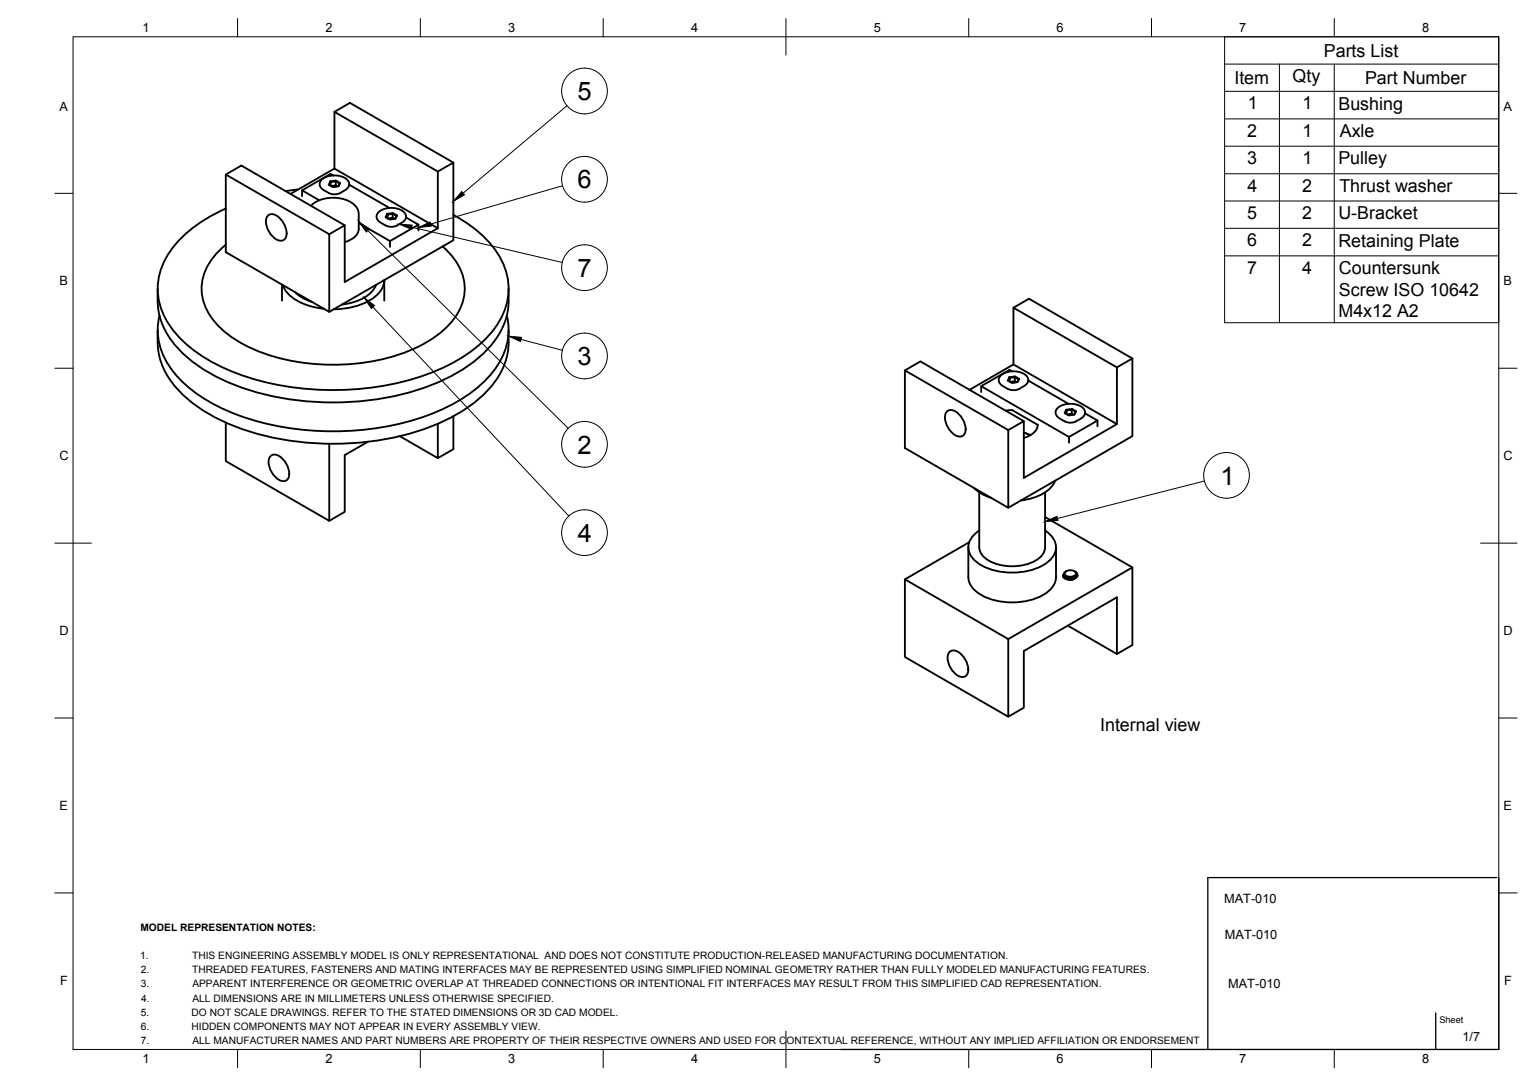
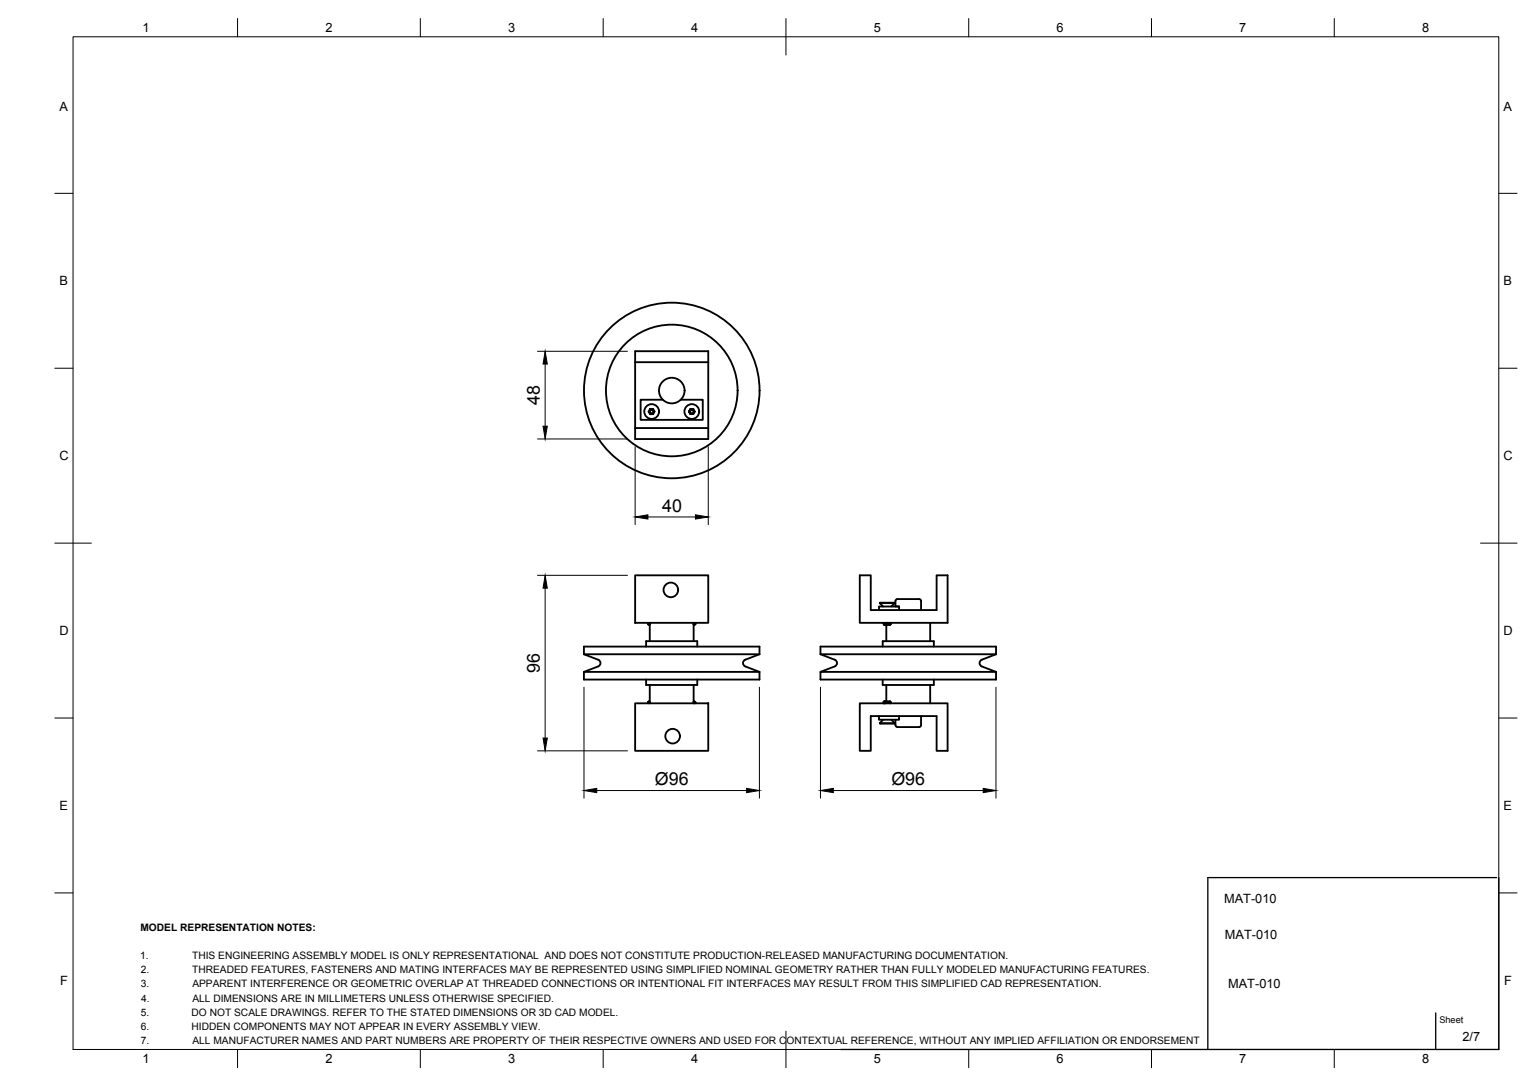
ISO-10303-21;
HEADER;
/* Generated by software containing ST-Developer
 * from STEP Tools, Inc. (www.steptools.com) 
 */

FILE_DESCRIPTION(
/* description */ ('STEP AP214'),
/* implementation_level */ '2;1');

FILE_NAME(
/* name */ 'MAT-010.step',
/* time_stamp */ '2026-11-14T05:50:49-08:00',
/* author */ (''),
/* organization */ (''),
/* preprocessor_version */ 'ST-DEVELOPER v20.2',
/* originating_system */ 'Autodesk Translation Framework v15.17.0.0',
/* authorisation */ '');

FILE_SCHEMA (('AUTOMOTIVE_DESIGN { 1 0 10303 214 3 1 1 }'));
ENDSEC;

DATA;
#10=MECHANICAL_DESIGN_GEOMETRIC_PRESENTATION_REPRESENTATION('',(#157,#158,
#159,#160,#161,#162,#163),#9903);
#11=ITEM_DEFINED_TRANSFORMATION($,$,#2108,#2305);
#12=ITEM_DEFINED_TRANSFORMATION($,$,#2117,#2306);
#13=ITEM_DEFINED_TRANSFORMATION($,$,#2141,#2307);
#14=ITEM_DEFINED_TRANSFORMATION($,$,#2189,#2308);
#15=ITEM_DEFINED_TRANSFORMATION($,$,#2198,#2309);
#16=ITEM_DEFINED_TRANSFORMATION($,$,#2221,#2310);
#17=ITEM_DEFINED_TRANSFORMATION($,$,#2234,#2311);
#18=ITEM_DEFINED_TRANSFORMATION($,$,#2189,#2312);
#19=ITEM_DEFINED_TRANSFORMATION($,$,#2198,#2313);
#20=ITEM_DEFINED_TRANSFORMATION($,$,#2221,#2314);
#21=ITEM_DEFINED_TRANSFORMATION($,$,#2234,#2315);
#22=ITEM_DEFINED_TRANSFORMATION($,$,#2234,#2316);
#23=ITEM_DEFINED_TRANSFORMATION($,$,#2234,#2317);
#24=(
REPRESENTATION_RELATIONSHIP($,$,#9938,#9937)
REPRESENTATION_RELATIONSHIP_WITH_TRANSFORMATION(#11)
SHAPE_REPRESENTATION_RELATIONSHIP()
);
#25=(
REPRESENTATION_RELATIONSHIP($,$,#9939,#9937)
REPRESENTATION_RELATIONSHIP_WITH_TRANSFORMATION(#12)
SHAPE_REPRESENTATION_RELATIONSHIP()
);
#26=(
REPRESENTATION_RELATIONSHIP($,$,#9940,#9937)
REPRESENTATION_RELATIONSHIP_WITH_TRANSFORMATION(#13)
SHAPE_REPRESENTATION_RELATIONSHIP()
);
#27=(
REPRESENTATION_RELATIONSHIP($,$,#9941,#9937)
REPRESENTATION_RELATIONSHIP_WITH_TRANSFORMATION(#14)
SHAPE_REPRESENTATION_RELATIONSHIP()
);
#28=(
REPRESENTATION_RELATIONSHIP($,$,#9942,#9937)
REPRESENTATION_RELATIONSHIP_WITH_TRANSFORMATION(#15)
SHAPE_REPRESENTATION_RELATIONSHIP()
);
#29=(
REPRESENTATION_RELATIONSHIP($,$,#9943,#9937)
REPRESENTATION_RELATIONSHIP_WITH_TRANSFORMATION(#16)
SHAPE_REPRESENTATION_RELATIONSHIP()
);
#30=(
REPRESENTATION_RELATIONSHIP($,$,#9944,#9937)
REPRESENTATION_RELATIONSHIP_WITH_TRANSFORMATION(#17)
SHAPE_REPRESENTATION_RELATIONSHIP()
);
#31=(
REPRESENTATION_RELATIONSHIP($,$,#9941,#9937)
REPRESENTATION_RELATIONSHIP_WITH_TRANSFORMATION(#18)
SHAPE_REPRESENTATION_RELATIONSHIP()
);
#32=(
REPRESENTATION_RELATIONSHIP($,$,#9942,#9937)
REPRESENTATION_RELATIONSHIP_WITH_TRANSFORMATION(#19)
SHAPE_REPRESENTATION_RELATIONSHIP()
);
#33=(
REPRESENTATION_RELATIONSHIP($,$,#9943,#9937)
REPRESENTATION_RELATIONSHIP_WITH_TRANSFORMATION(#20)
SHAPE_REPRESENTATION_RELATIONSHIP()
);
#34=(
REPRESENTATION_RELATIONSHIP($,$,#9944,#9937)
REPRESENTATION_RELATIONSHIP_WITH_TRANSFORMATION(#21)
SHAPE_REPRESENTATION_RELATIONSHIP()
);
#35=(
REPRESENTATION_RELATIONSHIP($,$,#9944,#9937)
REPRESENTATION_RELATIONSHIP_WITH_TRANSFORMATION(#22)
SHAPE_REPRESENTATION_RELATIONSHIP()
);
#36=(
REPRESENTATION_RELATIONSHIP($,$,#9944,#9937)
REPRESENTATION_RELATIONSHIP_WITH_TRANSFORMATION(#23)
SHAPE_REPRESENTATION_RELATIONSHIP()
);
#37=CONTEXT_DEPENDENT_SHAPE_REPRESENTATION(#24,#9924);
#38=CONTEXT_DEPENDENT_SHAPE_REPRESENTATION(#25,#9925);
#39=CONTEXT_DEPENDENT_SHAPE_REPRESENTATION(#26,#9926);
#40=CONTEXT_DEPENDENT_SHAPE_REPRESENTATION(#27,#9927);
#41=CONTEXT_DEPENDENT_SHAPE_REPRESENTATION(#28,#9928);
#42=CONTEXT_DEPENDENT_SHAPE_REPRESENTATION(#29,#9929);
#43=CONTEXT_DEPENDENT_SHAPE_REPRESENTATION(#30,#9930);
#44=CONTEXT_DEPENDENT_SHAPE_REPRESENTATION(#31,#9931);
#45=CONTEXT_DEPENDENT_SHAPE_REPRESENTATION(#32,#9932);
#46=CONTEXT_DEPENDENT_SHAPE_REPRESENTATION(#33,#9933);
#47=CONTEXT_DEPENDENT_SHAPE_REPRESENTATION(#34,#9934);
#48=CONTEXT_DEPENDENT_SHAPE_REPRESENTATION(#35,#9935);
#49=CONTEXT_DEPENDENT_SHAPE_REPRESENTATION(#36,#9936);
#50=NEXT_ASSEMBLY_USAGE_OCCURRENCE('Bushing:1','Bushing:1','Bushing:1',
#9946,#9947,'Bushing:1');
#51=NEXT_ASSEMBLY_USAGE_OCCURRENCE('Axle:1','Axle:1','Axle:1',#9946,#9948,
'Axle:1');
#52=NEXT_ASSEMBLY_USAGE_OCCURRENCE('Pulley:1','Pulley:1','Pulley:1',#9946,
#9949,'Pulley:1');
#53=NEXT_ASSEMBLY_USAGE_OCCURRENCE('Thrust Washer:1','Thrust Washer:1',
'Thrust Washer:1',#9946,#9950,'Thrust Washer:1');
#54=NEXT_ASSEMBLY_USAGE_OCCURRENCE('U-Bracket:1','U-Bracket:1',
'U-Bracket:1',#9946,#9951,'U-Bracket:1');
#55=NEXT_ASSEMBLY_USAGE_OCCURRENCE('Retaining Plate:1',
'Retaining Plate:1','Retaining Plate:1',#9946,#9952,'Retaining Plate:1');
#56=NEXT_ASSEMBLY_USAGE_OCCURRENCE(
'Countersunk Screw ISO 10642 M4x12 A2:1',
'Countersunk Screw ISO 10642 M4x12 A2:1',
'Countersunk Screw ISO 10642 M4x12 A2:1',#9946,#9953,
'Countersunk Screw ISO 10642 M4x12 A2:1');
#57=NEXT_ASSEMBLY_USAGE_OCCURRENCE('Thrust Washer:2','Thrust Washer:2',
'Thrust Washer:2',#9946,#9950,'Thrust Washer:2');
#58=NEXT_ASSEMBLY_USAGE_OCCURRENCE('U-Bracket:2','U-Bracket:2',
'U-Bracket:2',#9946,#9951,'U-Bracket:2');
#59=NEXT_ASSEMBLY_USAGE_OCCURRENCE('Retaining Plate:2',
'Retaining Plate:2','Retaining Plate:2',#9946,#9952,'Retaining Plate:2');
#60=NEXT_ASSEMBLY_USAGE_OCCURRENCE(
'Countersunk Screw ISO 10642 M4x12 A2:2',
'Countersunk Screw ISO 10642 M4x12 A2:2',
'Countersunk Screw ISO 10642 M4x12 A2:2',#9946,#9953,
'Countersunk Screw ISO 10642 M4x12 A2:2');
#61=NEXT_ASSEMBLY_USAGE_OCCURRENCE(
'Countersunk Screw ISO 10642 M4x12 A2:3',
'Countersunk Screw ISO 10642 M4x12 A2:3',
'Countersunk Screw ISO 10642 M4x12 A2:3',#9946,#9953,
'Countersunk Screw ISO 10642 M4x12 A2:3');
#62=NEXT_ASSEMBLY_USAGE_OCCURRENCE(
'Countersunk Screw ISO 10642 M4x12 A2:4',
'Countersunk Screw ISO 10642 M4x12 A2:4',
'Countersunk Screw ISO 10642 M4x12 A2:4',#9946,#9953,
'Countersunk Screw ISO 10642 M4x12 A2:4');
#63=(
BOUNDED_SURFACE()
B_SPLINE_SURFACE(1,2,((#4642,#4643,#4644,#4645,#4646,#4647,#4648,#4649,
#4650,#4651,#4652,#4653,#4654,#4655,#4656,#4657,#4658,#4659,#4660,#4661,
#4662,#4663,#4664,#4665,#4666,#4667,#4668,#4669,#4670,#4671,#4672,#4673,
#4674,#4675,#4676,#4677,#4678,#4679,#4680,#4681,#4682,#4683,#4684,#4685,
#4686,#4687,#4688,#4689,#4690,#4691,#4692,#4693,#4694,#4695,#4696,#4697,
#4698,#4699,#4700,#4701,#4702,#4703,#4704,#4705,#4706,#4707,#4708,#4709,
#4710,#4711,#4712,#4713,#4714,#4715,#4716,#4717,#4718,#4719,#4720,#4721,
#4722,#4723,#4724,#4725,#4726,#4727,#4728,#4729,#4730,#4731,#4732,#4733,
#4734,#4735,#4736,#4737,#4738,#4739,#4740,#4741,#4742,#4743,#4744,#4745,
#4746,#4747,#4748,#4749,#4750,#4751,#4752,#4753,#4754,#4755,#4756,#4757,
#4758,#4759,#4760,#4761,#4762,#4763,#4764,#4765,#4766,#4767,#4768,#4769,
#4770,#4771,#4772,#4773,#4774,#4775,#4776,#4777,#4778,#4779,#4780,#4781,
#4782,#4783,#4784,#4785,#4786,#4787,#4788,#4789,#4790,#4791,#4792,#4793,
#4794,#4795,#4796,#4797,#4798,#4799,#4800,#4801,#4802,#4803,#4804,#4805,
#4806,#4807,#4808,#4809,#4810,#4811,#4812,#4813,#4814,#4815,#4816,#4817,
#4818,#4819,#4820,#4821,#4822,#4823,#4824,#4825,#4826,#4827,#4828,#4829,
#4830,#4831,#4832,#4833,#4834,#4835,#4836,#4837,#4838,#4839,#4840,#4841,
#4842,#4843,#4844,#4845,#4846,#4847,#4848,#4849,#4850,#4851,#4852,#4853,
#4854,#4855,#4856,#4857,#4858,#4859,#4860,#4861,#4862,#4863,#4864,#4865,
#4866,#4867,#4868,#4869,#4870,#4871,#4872,#4873,#4874,#4875,#4876,#4877,
#4878,#4879,#4880,#4881,#4882,#4883,#4884,#4885,#4886,#4887,#4888,#4889,
#4890,#4891,#4892,#4893,#4894,#4895,#4896,#4897,#4898,#4899,#4900,#4901,
#4902,#4903,#4904,#4905,#4906,#4907,#4908,#4909,#4910,#4911,#4912,#4913,
#4914,#4915,#4916,#4917,#4918,#4919,#4920,#4921,#4922,#4923,#4924,#4925,
#4926,#4927,#4928,#4929,#4930,#4931,#4932,#4933,#4934,#4935,#4936,#4937,
#4938,#4939,#4940,#4941,#4942,#4943,#4944,#4945,#4946,#4947,#4948,#4949,
#4950,#4951,#4952,#4953,#4954,#4955,#4956,#4957,#4958,#4959,#4960,#4961,
#4962,#4963,#4964,#4965,#4966,#4967,#4968,#4969,#4970,#4971,#4972,#4973,
#4974,#4975,#4976,#4977,#4978,#4979,#4980,#4981,#4982,#4983,#4984,#4985,
#4986,#4987,#4988,#4989,#4990,#4991,#4992,#4993,#4994,#4995,#4996,#4997,
#4998,#4999,#5000,#5001,#5002,#5003,#5004,#5005,#5006,#5007,#5008,#5009,
#5010,#5011,#5012,#5013,#5014,#5015,#5016,#5017,#5018,#5019,#5020,#5021,
#5022,#5023,#5024,#5025,#5026,#5027,#5028,#5029,#5030,#5031,#5032,#5033,
#5034,#5035,#5036,#5037,#5038,#5039,#5040,#5041,#5042,#5043,#5044,#5045,
#5046,#5047,#5048,#5049,#5050,#5051,#5052,#5053,#5054,#5055,#5056,#5057,
#5058,#5059,#5060,#5061,#5062,#5063,#5064,#5065,#5066,#5067,#5068,#5069,
#5070,#5071,#5072,#5073,#5074,#5075,#5076,#5077,#5078,#5079,#5080,#5081,
#5082,#5083,#5084,#5085,#5086,#5087,#5088,#5089,#5090,#5091,#5092,#5093,
#5094,#5095,#5096,#5097,#5098,#5099,#5100,#5101,#5102,#5103,#5104,#5105,
#5106,#5107,#5108,#5109,#5110,#5111,#5112,#5113,#5114,#5115,#5116,#5117,
#5118,#5119,#5120,#5121,#5122,#5123,#5124,#5125,#5126,#5127,#5128,#5129,
#5130,#5131,#5132,#5133,#5134,#5135,#5136,#5137,#5138,#5139,#5140,#5141,
#5142,#5143,#5144,#5145,#5146,#5147,#5148,#5149,#5150,#5151,#5152,#5153,
#5154,#5155,#5156,#5157,#5158,#5159,#5160,#5161,#5162,#5163,#5164,#5165,
#5166,#5167,#5168,#5169,#5170,#5171,#5172,#5173,#5174,#5175,#5176,#5177,
#5178,#5179,#5180,#5181,#5182,#5183,#5184,#5185,#5186,#5187,#5188,#5189,
#5190,#5191,#5192,#5193,#5194,#5195,#5196,#5197,#5198,#5199,#5200,#5201,
#5202,#5203,#5204,#5205,#5206,#5207,#5208,#5209,#5210,#5211,#5212,#5213,
#5214,#5215,#5216,#5217,#5218,#5219,#5220,#5221,#5222,#5223,#5224,#5225,
#5226,#5227,#5228,#5229,#5230,#5231,#5232,#5233,#5234,#5235,#5236,#5237,
#5238,#5239,#5240,#5241,#5242,#5243,#5244,#5245,#5246,#5247,#5248,#5249,
#5250,#5251,#5252,#5253,#5254,#5255,#5256,#5257,#5258,#5259,#5260,#5261,
#5262,#5263,#5264,#5265,#5266,#5267,#5268,#5269,#5270,#5271,#5272,#5273,
#5274,#5275,#5276,#5277,#5278,#5279,#5280,#5281,#5282,#5283,#5284,#5285,
#5286,#5287,#5288,#5289,#5290,#5291,#5292,#5293,#5294,#5295,#5296,#5297,
#5298,#5299,#5300,#5301,#5302,#5303,#5304,#5305,#5306,#5307,#5308,#5309,
#5310,#5311,#5312,#5313,#5314,#5315,#5316,#5317,#5318,#5319,#5320,#5321,
#5322,#5323,#5324,#5325,#5326,#5327,#5328,#5329,#5330,#5331,#5332,#5333,
#5334,#5335,#5336,#5337,#5338,#5339,#5340,#5341,#5342,#5343,#5344,#5345,
#5346,#5347,#5348,#5349,#5350,#5351,#5352,#5353,#5354,#5355,#5356,#5357,
#5358,#5359,#5360,#5361,#5362,#5363,#5364,#5365,#5366,#5367,#5368,#5369,
#5370,#5371,#5372,#5373,#5374,#5375,#5376,#5377,#5378,#5379,#5380,#5381,
#5382,#5383,#5384,#5385,#5386,#5387,#5388,#5389,#5390,#5391,#5392,#5393,
#5394,#5395,#5396,#5397,#5398,#5399,#5400,#5401,#5402,#5403,#5404,#5405,
#5406,#5407,#5408,#5409,#5410,#5411,#5412,#5413,#5414,#5415,#5416,#5417,
#5418,#5419,#5420,#5421,#5422,#5423,#5424,#5425,#5426,#5427,#5428,#5429,
#5430,#5431,#5432,#5433,#5434,#5435,#5436,#5437,#5438,#5439,#5440,#5441,
#5442,#5443,#5444,#5445,#5446,#5447,#5448,#5449,#5450,#5451,#5452,#5453,
#5454,#5455,#5456,#5457,#5458,#5459,#5460,#5461,#5462,#5463,#5464,#5465,
#5466,#5467,#5468,#5469,#5470,#5471,#5472,#5473,#5474,#5475,#5476,#5477,
#5478,#5479,#5480,#5481,#5482,#5483,#5484,#5485,#5486,#5487,#5488,#5489,
#5490,#5491,#5492,#5493,#5494,#5495,#5496,#5497,#5498,#5499,#5500,#5501,
#5502,#5503,#5504,#5505,#5506,#5507,#5508,#5509,#5510,#5511,#5512,#5513,
#5514,#5515,#5516,#5517,#5518,#5519,#5520,#5521,#5522,#5523,#5524,#5525,
#5526,#5527,#5528,#5529,#5530,#5531,#5532,#5533,#5534,#5535,#5536,#5537,
#5538,#5539,#5540,#5541,#5542,#5543,#5544,#5545,#5546,#5547,#5548,#5549,
#5550,#5551,#5552,#5553,#5554,#5555,#5556,#5557,#5558,#5559,#5560,#5561,
#5562,#5563,#5564,#5565,#5566,#5567,#5568,#5569,#5570,#5571,#5572,#5573,
#5574,#5575,#5576,#5577,#5578,#5579,#5580,#5581,#5582,#5583,#5584,#5585,
#5586,#5587,#5588,#5589,#5590,#5591,#5592,#5593,#5594,#5595,#5596,#5597,
#5598,#5599,#5600,#5601,#5602,#5603,#5604,#5605,#5606,#5607,#5608,#5609,
#5610,#5611,#5612,#5613,#5614,#5615,#5616,#5617,#5618,#5619,#5620,#5621,
#5622,#5623,#5624,#5625,#5626,#5627,#5628,#5629,#5630,#5631,#5632,#5633,
#5634,#5635,#5636,#5637,#5638,#5639,#5640,#5641,#5642,#5643,#5644,#5645,
#5646,#5647,#5648,#5649,#5650,#5651,#5652,#5653,#5654,#5655,#5656,#5657,
#5658,#5659,#5660,#5661,#5662,#5663,#5664,#5665,#5666,#5667,#5668,#5669,
#5670,#5671,#5672,#5673,#5674,#5675,#5676,#5677,#5678,#5679,#5680,#5681,
#5682,#5683,#5684,#5685,#5686,#5687,#5688,#5689,#5690,#5691,#5692,#5693,
#5694,#5695,#5696,#5697,#5698,#5699,#5700,#5701,#5702,#5703,#5704,#5705,
#5706,#5707,#5708,#5709,#5710,#5711,#5712,#5713,#5714,#5715,#5716,#5717,
#5718,#5719,#5720,#5721,#5722,#5723,#5724,#5725,#5726,#5727,#5728,#5729,
#5730,#5731,#5732,#5733,#5734,#5735,#5736,#5737,#5738,#5739,#5740,#5741,
#5742,#5743,#5744,#5745,#5746,#5747,#5748,#5749,#5750,#5751,#5752,#5753,
#5754,#5755,#5756,#5757,#5758,#5759,#5760,#5761,#5762,#5763,#5764,#5765,
#5766,#5767,#5768,#5769,#5770,#5771,#5772,#5773,#5774,#5775,#5776,#5777,
#5778,#5779,#5780,#5781,#5782,#5783,#5784,#5785,#5786,#5787,#5788,#5789,
#5790,#5791,#5792,#5793,#5794,#5795,#5796,#5797,#5798,#5799,#5800,#5801,
#5802,#5803,#5804,#5805,#5806,#5807,#5808,#5809,#5810,#5811,#5812,#5813,
#5814,#5815,#5816,#5817,#5818,#5819,#5820,#5821,#5822,#5823,#5824,#5825,
#5826,#5827,#5828,#5829,#5830,#5831,#5832,#5833,#5834,#5835,#5836,#5837,
#5838,#5839,#5840,#5841,#5842,#5843,#5844,#5845,#5846,#5847,#5848,#5849,
#5850,#5851,#5852,#5853,#5854,#5855,#5856,#5857,#5858,#5859,#5860,#5861,
#5862,#5863,#5864,#5865,#5866,#5867,#5868,#5869,#5870,#5871,#5872,#5873,
#5874,#5875,#5876,#5877,#5878,#5879,#5880,#5881,#5882,#5883,#5884,#5885,
#5886,#5887,#5888,#5889,#5890,#5891,#5892,#5893,#5894,#5895,#5896,#5897,
#5898,#5899,#5900,#5901,#5902,#5903,#5904,#5905,#5906,#5907,#5908,#5909,
#5910,#5911,#5912),(#5913,#5914,#5915,#5916,#5917,#5918,#5919,#5920,#5921,
#5922,#5923,#5924,#5925,#5926,#5927,#5928,#5929,#5930,#5931,#5932,#5933,
#5934,#5935,#5936,#5937,#5938,#5939,#5940,#5941,#5942,#5943,#5944,#5945,
#5946,#5947,#5948,#5949,#5950,#5951,#5952,#5953,#5954,#5955,#5956,#5957,
#5958,#5959,#5960,#5961,#5962,#5963,#5964,#5965,#5966,#5967,#5968,#5969,
#5970,#5971,#5972,#5973,#5974,#5975,#5976,#5977,#5978,#5979,#5980,#5981,
#5982,#5983,#5984,#5985,#5986,#5987,#5988,#5989,#5990,#5991,#5992,#5993,
#5994,#5995,#5996,#5997,#5998,#5999,#6000,#6001,#6002,#6003,#6004,#6005,
#6006,#6007,#6008,#6009,#6010,#6011,#6012,#6013,#6014,#6015,#6016,#6017,
#6018,#6019,#6020,#6021,#6022,#6023,#6024,#6025,#6026,#6027,#6028,#6029,
#6030,#6031,#6032,#6033,#6034,#6035,#6036,#6037,#6038,#6039,#6040,#6041,
#6042,#6043,#6044,#6045,#6046,#6047,#6048,#6049,#6050,#6051,#6052,#6053,
#6054,#6055,#6056,#6057,#6058,#6059,#6060,#6061,#6062,#6063,#6064,#6065,
#6066,#6067,#6068,#6069,#6070,#6071,#6072,#6073,#6074,#6075,#6076,#6077,
#6078,#6079,#6080,#6081,#6082,#6083,#6084,#6085,#6086,#6087,#6088,#6089,
#6090,#6091,#6092,#6093,#6094,#6095,#6096,#6097,#6098,#6099,#6100,#6101,
#6102,#6103,#6104,#6105,#6106,#6107,#6108,#6109,#6110,#6111,#6112,#6113,
#6114,#6115,#6116,#6117,#6118,#6119,#6120,#6121,#6122,#6123,#6124,#6125,
#6126,#6127,#6128,#6129,#6130,#6131,#6132,#6133,#6134,#6135,#6136,#6137,
#6138,#6139,#6140,#6141,#6142,#6143,#6144,#6145,#6146,#6147,#6148,#6149,
#6150,#6151,#6152,#6153,#6154,#6155,#6156,#6157,#6158,#6159,#6160,#6161,
#6162,#6163,#6164,#6165,#6166,#6167,#6168,#6169,#6170,#6171,#6172,#6173,
#6174,#6175,#6176,#6177,#6178,#6179,#6180,#6181,#6182,#6183,#6184,#6185,
#6186,#6187,#6188,#6189,#6190,#6191,#6192,#6193,#6194,#6195,#6196,#6197,
#6198,#6199,#6200,#6201,#6202,#6203,#6204,#6205,#6206,#6207,#6208,#6209,
#6210,#6211,#6212,#6213,#6214,#6215,#6216,#6217,#6218,#6219,#6220,#6221,
#6222,#6223,#6224,#6225,#6226,#6227,#6228,#6229,#6230,#6231,#6232,#6233,
#6234,#6235,#6236,#6237,#6238,#6239,#6240,#6241,#6242,#6243,#6244,#6245,
#6246,#6247,#6248,#6249,#6250,#6251,#6252,#6253,#6254,#6255,#6256,#6257,
#6258,#6259,#6260,#6261,#6262,#6263,#6264,#6265,#6266,#6267,#6268,#6269,
#6270,#6271,#6272,#6273,#6274,#6275,#6276,#6277,#6278,#6279,#6280,#6281,
#6282,#6283,#6284,#6285,#6286,#6287,#6288,#6289,#6290,#6291,#6292,#6293,
#6294,#6295,#6296,#6297,#6298,#6299,#6300,#6301,#6302,#6303,#6304,#6305,
#6306,#6307,#6308,#6309,#6310,#6311,#6312,#6313,#6314,#6315,#6316,#6317,
#6318,#6319,#6320,#6321,#6322,#6323,#6324,#6325,#6326,#6327,#6328,#6329,
#6330,#6331,#6332,#6333,#6334,#6335,#6336,#6337,#6338,#6339,#6340,#6341,
#6342,#6343,#6344,#6345,#6346,#6347,#6348,#6349,#6350,#6351,#6352,#6353,
#6354,#6355,#6356,#6357,#6358,#6359,#6360,#6361,#6362,#6363,#6364,#6365,
#6366,#6367,#6368,#6369,#6370,#6371,#6372,#6373,#6374,#6375,#6376,#6377,
#6378,#6379,#6380,#6381,#6382,#6383,#6384,#6385,#6386,#6387,#6388,#6389,
#6390,#6391,#6392,#6393,#6394,#6395,#6396,#6397,#6398,#6399,#6400,#6401,
#6402,#6403,#6404,#6405,#6406,#6407,#6408,#6409,#6410,#6411,#6412,#6413,
#6414,#6415,#6416,#6417,#6418,#6419,#6420,#6421,#6422,#6423,#6424,#6425,
#6426,#6427,#6428,#6429,#6430,#6431,#6432,#6433,#6434,#6435,#6436,#6437,
#6438,#6439,#6440,#6441,#6442,#6443,#6444,#6445,#6446,#6447,#6448,#6449,
#6450,#6451,#6452,#6453,#6454,#6455,#6456,#6457,#6458,#6459,#6460,#6461,
#6462,#6463,#6464,#6465,#6466,#6467,#6468,#6469,#6470,#6471,#6472,#6473,
#6474,#6475,#6476,#6477,#6478,#6479,#6480,#6481,#6482,#6483,#6484,#6485,
#6486,#6487,#6488,#6489,#6490,#6491,#6492,#6493,#6494,#6495,#6496,#6497,
#6498,#6499,#6500,#6501,#6502,#6503,#6504,#6505,#6506,#6507,#6508,#6509,
#6510,#6511,#6512,#6513,#6514,#6515,#6516,#6517,#6518,#6519,#6520,#6521,
#6522,#6523,#6524,#6525,#6526,#6527,#6528,#6529,#6530,#6531,#6532,#6533,
#6534,#6535,#6536,#6537,#6538,#6539,#6540,#6541,#6542,#6543,#6544,#6545,
#6546,#6547,#6548,#6549,#6550,#6551,#6552,#6553,#6554,#6555,#6556,#6557,
#6558,#6559,#6560,#6561,#6562,#6563,#6564,#6565,#6566,#6567,#6568,#6569,
#6570,#6571,#6572,#6573,#6574,#6575,#6576,#6577,#6578,#6579,#6580,#6581,
#6582,#6583,#6584,#6585,#6586,#6587,#6588,#6589,#6590,#6591,#6592,#6593,
#6594,#6595,#6596,#6597,#6598,#6599,#6600,#6601,#6602,#6603,#6604,#6605,
#6606,#6607,#6608,#6609,#6610,#6611,#6612,#6613,#6614,#6615,#6616,#6617,
#6618,#6619,#6620,#6621,#6622,#6623,#6624,#6625,#6626,#6627,#6628,#6629,
#6630,#6631,#6632,#6633,#6634,#6635,#6636,#6637,#6638,#6639,#6640,#6641,
#6642,#6643,#6644,#6645,#6646,#6647,#6648,#6649,#6650,#6651,#6652,#6653,
#6654,#6655,#6656,#6657,#6658,#6659,#6660,#6661,#6662,#6663,#6664,#6665,
#6666,#6667,#6668,#6669,#6670,#6671,#6672,#6673,#6674,#6675,#6676,#6677,
#6678,#6679,#6680,#6681,#6682,#6683,#6684,#6685,#6686,#6687,#6688,#6689,
#6690,#6691,#6692,#6693,#6694,#6695,#6696,#6697,#6698,#6699,#6700,#6701,
#6702,#6703,#6704,#6705,#6706,#6707,#6708,#6709,#6710,#6711,#6712,#6713,
#6714,#6715,#6716,#6717,#6718,#6719,#6720,#6721,#6722,#6723,#6724,#6725,
#6726,#6727,#6728,#6729,#6730,#6731,#6732,#6733,#6734,#6735,#6736,#6737,
#6738,#6739,#6740,#6741,#6742,#6743,#6744,#6745,#6746,#6747,#6748,#6749,
#6750,#6751,#6752,#6753,#6754,#6755,#6756,#6757,#6758,#6759,#6760,#6761,
#6762,#6763,#6764,#6765,#6766,#6767,#6768,#6769,#6770,#6771,#6772,#6773,
#6774,#6775,#6776,#6777,#6778,#6779,#6780,#6781,#6782,#6783,#6784,#6785,
#6786,#6787,#6788,#6789,#6790,#6791,#6792,#6793,#6794,#6795,#6796,#6797,
#6798,#6799,#6800,#6801,#6802,#6803,#6804,#6805,#6806,#6807,#6808,#6809,
#6810,#6811,#6812,#6813,#6814,#6815,#6816,#6817,#6818,#6819,#6820,#6821,
#6822,#6823,#6824,#6825,#6826,#6827,#6828,#6829,#6830,#6831,#6832,#6833,
#6834,#6835,#6836,#6837,#6838,#6839,#6840,#6841,#6842,#6843,#6844,#6845,
#6846,#6847,#6848,#6849,#6850,#6851,#6852,#6853,#6854,#6855,#6856,#6857,
#6858,#6859,#6860,#6861,#6862,#6863,#6864,#6865,#6866,#6867,#6868,#6869,
#6870,#6871,#6872,#6873,#6874,#6875,#6876,#6877,#6878,#6879,#6880,#6881,
#6882,#6883,#6884,#6885,#6886,#6887,#6888,#6889,#6890,#6891,#6892,#6893,
#6894,#6895,#6896,#6897,#6898,#6899,#6900,#6901,#6902,#6903,#6904,#6905,
#6906,#6907,#6908,#6909,#6910,#6911,#6912,#6913,#6914,#6915,#6916,#6917,
#6918,#6919,#6920,#6921,#6922,#6923,#6924,#6925,#6926,#6927,#6928,#6929,
#6930,#6931,#6932,#6933,#6934,#6935,#6936,#6937,#6938,#6939,#6940,#6941,
#6942,#6943,#6944,#6945,#6946,#6947,#6948,#6949,#6950,#6951,#6952,#6953,
#6954,#6955,#6956,#6957,#6958,#6959,#6960,#6961,#6962,#6963,#6964,#6965,
#6966,#6967,#6968,#6969,#6970,#6971,#6972,#6973,#6974,#6975,#6976,#6977,
#6978,#6979,#6980,#6981,#6982,#6983,#6984,#6985,#6986,#6987,#6988,#6989,
#6990,#6991,#6992,#6993,#6994,#6995,#6996,#6997,#6998,#6999,#7000,#7001,
#7002,#7003,#7004,#7005,#7006,#7007,#7008,#7009,#7010,#7011,#7012,#7013,
#7014,#7015,#7016,#7017,#7018,#7019,#7020,#7021,#7022,#7023,#7024,#7025,
#7026,#7027,#7028,#7029,#7030,#7031,#7032,#7033,#7034,#7035,#7036,#7037,
#7038,#7039,#7040,#7041,#7042,#7043,#7044,#7045,#7046,#7047,#7048,#7049,
#7050,#7051,#7052,#7053,#7054,#7055,#7056,#7057,#7058,#7059,#7060,#7061,
#7062,#7063,#7064,#7065,#7066,#7067,#7068,#7069,#7070,#7071,#7072,#7073,
#7074,#7075,#7076,#7077,#7078,#7079,#7080,#7081,#7082,#7083,#7084,#7085,
#7086,#7087,#7088,#7089,#7090,#7091,#7092,#7093,#7094,#7095,#7096,#7097,
#7098,#7099,#7100,#7101,#7102,#7103,#7104,#7105,#7106,#7107,#7108,#7109,
#7110,#7111,#7112,#7113,#7114,#7115,#7116,#7117,#7118,#7119,#7120,#7121,
#7122,#7123,#7124,#7125,#7126,#7127,#7128,#7129,#7130,#7131,#7132,#7133,
#7134,#7135,#7136,#7137,#7138,#7139,#7140,#7141,#7142,#7143,#7144,#7145,
#7146,#7147,#7148,#7149,#7150,#7151,#7152,#7153,#7154,#7155,#7156,#7157,
#7158,#7159,#7160,#7161,#7162,#7163,#7164,#7165,#7166,#7167,#7168,#7169,
#7170,#7171,#7172,#7173,#7174,#7175,#7176,#7177,#7178,#7179,#7180,#7181,
#7182,#7183)),.UNSPECIFIED.,.F.,.F.,.F.)
B_SPLINE_SURFACE_WITH_KNOTS((2,2),(3,2,2,2,2,2,2,2,2,2,2,2,2,2,2,2,2,2,
2,2,2,2,2,2,2,2,2,2,2,2,2,2,2,2,2,2,2,2,2,2,2,2,2,2,2,2,2,2,2,2,2,2,2,2,
2,2,2,2,2,2,2,2,2,2,2,2,2,2,2,2,2,2,2,2,2,2,2,2,2,2,2,2,2,2,2,2,2,2,2,2,
2,2,2,2,2,2,2,2,2,2,2,2,2,2,2,2,2,2,2,2,2,2,2,2,2,2,2,2,2,2,2,2,2,2,2,2,
2,2,2,2,2,2,2,2,2,2,2,2,2,2,2,2,2,2,2,2,2,2,2,2,2,2,2,2,2,2,2,2,2,2,2,2,
2,2,2,2,2,2,2,2,2,2,2,2,2,2,2,2,2,2,2,2,2,2,2,2,2,2,2,2,2,2,2,2,2,2,2,2,
2,2,2,2,2,2,2,2,2,2,2,2,2,2,2,2,2,2,2,2,2,2,2,2,2,2,2,2,2,2,2,2,2,2,2,2,
2,2,2,2,2,2,2,2,2,2,2,2,2,2,2,2,2,2,2,2,2,2,2,2,2,2,2,2,2,2,2,2,2,2,2,2,
2,2,2,2,2,2,2,2,2,2,2,2,2,2,2,2,2,2,2,2,2,2,2,2,2,2,2,2,2,2,2,2,2,2,2,2,
2,2,2,2,2,2,2,2,2,2,2,2,2,2,2,2,2,2,2,2,2,2,2,2,2,2,2,2,2,2,2,2,2,2,2,2,
2,2,2,2,2,2,2,2,2,2,2,2,2,2,2,2,2,2,2,2,2,2,2,2,2,2,2,2,2,2,2,2,2,2,2,2,
2,2,2,2,2,2,2,2,2,2,2,2,2,2,2,2,2,2,2,2,2,2,2,2,2,2,2,2,2,2,2,2,2,2,2,2,
2,2,2,2,2,2,2,2,2,2,2,2,2,2,2,2,2,2,2,2,2,2,2,2,2,2,2,2,2,2,2,2,2,2,2,2,
2,2,2,2,2,2,2,2,2,2,2,2,2,2,2,2,2,2,2,2,2,2,2,2,2,2,2,2,2,2,2,2,2,2,2,2,
2,2,2,2,2,2,2,2,2,2,2,2,2,2,2,2,2,2,2,2,2,2,2,2,2,2,2,2,2,2,2,2,2,2,2,2,
2,2,2,2,2,2,2,2,2,2,2,2,2,2,2,2,2,2,2,2,2,2,2,2,2,2,2,2,2,2,2,2,2,2,2,2,
2,2,2,2,2,2,2,2,2,2,2,2,2,2,2,2,2,2,2,2,2,2,2,2,2,2,2,2,2,2,2,2,2,2,2,2,
2,2,2,2,2,2,2,2,2,2,2,2,2,2,2,2,2,2,2,2,2,2,2,2,2,2,2,2,2,2,2,2,2,2,2,2,
2,2,2,2,2,3),(0.,1.0000000013075),(0.,0.00157232704402516,0.00314465408805031,
0.00471698113207547,0.00628930817610063,0.00786163522012579,0.00943396226415094,
0.0110062893081761,0.0125786163522013,0.0141509433962264,0.0157232704402516,
0.0172955974842767,0.0188679245283019,0.020440251572327,0.0220125786163522,
0.0235849056603774,0.0251572327044025,0.0267295597484277,0.0283018867924528,
0.029874213836478,0.0314465408805031,0.0330188679245283,0.0345911949685535,
0.0361635220125786,0.0377358490566038,0.0393081761006289,0.0408805031446541,
0.0424528301886792,0.0440251572327044,0.0455974842767296,0.0471698113207547,
0.0487421383647799,0.050314465408805,0.0518867924528302,0.0534591194968553,
0.0550314465408805,0.0566037735849057,0.0581761006289308,0.059748427672956,
0.0613207547169811,0.0628930817610063,0.0644654088050314,0.0660377358490566,
0.0676100628930818,0.0691823899371069,0.0707547169811321,0.0723270440251572,
0.0738993710691824,0.0754716981132075,0.0770440251572327,0.0786163522012579,
0.080188679245283,0.0817610062893082,0.0833333333333333,0.0849056603773585,
0.0864779874213836,0.0880503144654088,0.089622641509434,0.0911949685534591,
0.0927672955974843,0.0943396226415094,0.0959119496855346,0.0974842767295598,
0.0990566037735849,0.10062893081761,0.102201257861635,0.10377358490566,
0.105345911949686,0.106918238993711,0.108490566037736,0.110062893081761,
0.111635220125786,0.113207547169811,0.114779874213836,0.116352201257862,
0.117924528301887,0.119496855345912,0.121069182389937,0.122641509433962,
0.124213836477987,0.125786163522013,0.127358490566038,0.128930817610063,
0.130503144654088,0.132075471698113,0.133647798742138,0.135220125786164,
0.136792452830189,0.138364779874214,0.139937106918239,0.141509433962264,
0.143081761006289,0.144654088050314,0.14622641509434,0.147798742138365,
0.14937106918239,0.150943396226415,0.15251572327044,0.154088050314465,0.155660377358491,
0.157232704402516,0.158805031446541,0.160377358490566,0.161949685534591,
0.163522012578616,0.165094339622642,0.166666666666667,0.168238993710692,
0.169811320754717,0.171383647798742,0.172955974842767,0.174528301886792,
0.176100628930818,0.177672955974843,0.179245283018868,0.180817610062893,
0.182389937106918,0.183962264150943,0.185534591194969,0.187106918238994,
0.188679245283019,0.190251572327044,0.191823899371069,0.193396226415094,
0.19496855345912,0.196540880503145,0.19811320754717,0.199685534591195,0.20125786163522,
0.202830188679245,0.20440251572327,0.205974842767296,0.207547169811321,
0.209119496855346,0.210691823899371,0.212264150943396,0.213836477987421,
0.215408805031447,0.216981132075472,0.218553459119497,0.220125786163522,
0.221698113207547,0.223270440251572,0.224842767295597,0.226415094339623,
0.227987421383648,0.229559748427673,0.231132075471698,0.232704402515723,
0.234276729559748,0.235849056603774,0.237421383647799,0.238993710691824,
0.240566037735849,0.242138364779874,0.243710691823899,0.245283018867925,
0.24685534591195,0.248427672955975,0.25,0.251572327044025,0.25314465408805,
0.254716981132075,0.256289308176101,0.257861635220126,0.259433962264151,
0.261006289308176,0.262578616352201,0.264150943396226,0.265723270440252,
0.267295597484277,0.268867924528302,0.270440251572327,0.272012578616352,
0.273584905660377,0.275157232704403,0.276729559748428,0.278301886792453,
0.279874213836478,0.281446540880503,0.283018867924528,0.284591194968553,
0.286163522012579,0.287735849056604,0.289308176100629,0.290880503144654,
0.292452830188679,0.294025157232704,0.29559748427673,0.297169811320755,
0.29874213836478,0.300314465408805,0.30188679245283,0.303459119496855,0.30503144654088,
0.306603773584906,0.308176100628931,0.309748427672956,0.311320754716981,
0.312893081761006,0.314465408805031,0.316037735849057,0.317610062893082,
0.319182389937107,0.320754716981132,0.322327044025157,0.323899371069182,
0.325471698113208,0.327044025157233,0.328616352201258,0.330188679245283,
0.331761006289308,0.333333333333333,0.334905660377358,0.336477987421384,
0.338050314465409,0.339622641509434,0.341194968553459,0.342767295597484,
0.344339622641509,0.345911949685535,0.34748427672956,0.349056603773585,
0.35062893081761,0.352201257861635,0.35377358490566,0.355345911949686,0.356918238993711,
0.358490566037736,0.360062893081761,0.361635220125786,0.363207547169811,
0.364779874213836,0.366352201257862,0.367924528301887,0.369496855345912,
0.371069182389937,0.372641509433962,0.374213836477987,0.375786163522013,
0.377358490566038,0.378930817610063,0.380503144654088,0.382075471698113,
0.383647798742138,0.385220125786164,0.386792452830189,0.388364779874214,
0.389937106918239,0.391509433962264,0.393081761006289,0.394654088050314,
0.39622641509434,0.397798742138365,0.39937106918239,0.400943396226415,0.40251572327044,
0.404088050314465,0.405660377358491,0.407232704402516,0.408805031446541,
0.410377358490566,0.411949685534591,0.413522012578616,0.415094339622642,
0.416666666666667,0.418238993710692,0.419811320754717,0.421383647798742,
0.422955974842767,0.424528301886792,0.426100628930818,0.427672955974843,
0.429245283018868,0.430817610062893,0.432389937106918,0.433962264150943,
0.435534591194969,0.437106918238994,0.438679245283019,0.440251572327044,
0.441823899371069,0.443396226415094,0.44496855345912,0.446540880503145,
0.44811320754717,0.449685534591195,0.45125786163522,0.452830188679245,0.45440251572327,
0.455974842767296,0.457547169811321,0.459119496855346,0.460691823899371,
0.462264150943396,0.463836477987421,0.465408805031447,0.466981132075472,
0.468553459119497,0.470125786163522,0.471698113207547,0.473270440251572,
0.474842767295597,0.476415094339623,0.477987421383648,0.479559748427673,
0.481132075471698,0.482704402515723,0.484276729559748,0.485849056603774,
0.487421383647799,0.488993710691824,0.490566037735849,0.492138364779874,
0.493710691823899,0.495283018867925,0.49685534591195,0.498427672955975,
0.5,0.501572327044025,0.50314465408805,0.504716981132076,0.506289308176101,
0.507861635220126,0.509433962264151,0.511006289308176,0.512578616352201,
0.514150943396226,0.515723270440252,0.517295597484277,0.518867924528302,
0.520440251572327,0.522012578616352,0.523584905660377,0.525157232704403,
0.526729559748428,0.528301886792453,0.529874213836478,0.531446540880503,
0.533018867924528,0.534591194968553,0.536163522012579,0.537735849056604,
0.539308176100629,0.540880503144654,0.542452830188679,0.544025157232704,
0.54559748427673,0.547169811320755,0.54874213836478,0.550314465408805,0.55188679245283,
0.553459119496855,0.555031446540881,0.556603773584906,0.558176100628931,
0.559748427672956,0.561320754716981,0.562893081761006,0.564465408805031,
0.566037735849057,0.567610062893082,0.569182389937107,0.570754716981132,
0.572327044025157,0.573899371069182,0.575471698113208,0.577044025157233,
0.578616352201258,0.580188679245283,0.581761006289308,0.583333333333333,
0.584905660377358,0.586477987421384,0.588050314465409,0.589622641509434,
0.591194968553459,0.592767295597484,0.594339622641509,0.595911949685535,
0.59748427672956,0.599056603773585,0.60062893081761,0.602201257861635,0.60377358490566,
0.605345911949686,0.606918238993711,0.608490566037736,0.610062893081761,
0.611635220125786,0.613207547169811,0.614779874213837,0.616352201257862,
0.617924528301887,0.619496855345912,0.621069182389937,0.622641509433962,
0.624213836477987,0.625786163522013,0.627358490566038,0.628930817610063,
0.630503144654088,0.632075471698113,0.633647798742138,0.635220125786163,
0.636792452830189,0.638364779874214,0.639937106918239,0.641509433962264,
0.643081761006289,0.644654088050314,0.64622641509434,0.647798742138365,
0.64937106918239,0.650943396226415,0.65251572327044,0.654088050314465,0.655660377358491,
0.657232704402516,0.658805031446541,0.660377358490566,0.661949685534591,
0.663522012578616,0.665094339622642,0.666666666666667,0.668238993710692,
0.669811320754717,0.671383647798742,0.672955974842767,0.674528301886792,
0.676100628930818,0.677672955974843,0.679245283018868,0.680817610062893,
0.682389937106918,0.683962264150943,0.685534591194969,0.687106918238994,
0.688679245283019,0.690251572327044,0.691823899371069,0.693396226415094,
0.694968553459119,0.696540880503145,0.69811320754717,0.699685534591195,
0.70125786163522,0.702830188679245,0.70440251572327,0.705974842767296,0.707547169811321,
0.709119496855346,0.710691823899371,0.712264150943396,0.713836477987421,
0.715408805031447,0.716981132075472,0.718553459119497,0.720125786163522,
0.721698113207547,0.723270440251572,0.724842767295597,0.726415094339623,
0.727987421383648,0.729559748427673,0.731132075471698,0.732704402515723,
0.734276729559748,0.735849056603774,0.737421383647799,0.738993710691824,
0.740566037735849,0.742138364779874,0.743710691823899,0.745283018867924,
0.74685534591195,0.748427672955975,0.75,0.751572327044025,0.75314465408805,
0.754716981132076,0.756289308176101,0.757861635220126,0.759433962264151,
0.761006289308176,0.762578616352201,0.764150943396226,0.765723270440252,
0.767295597484277,0.768867924528302,0.770440251572327,0.772012578616352,
0.773584905660377,0.775157232704403,0.776729559748428,0.778301886792453,
0.779874213836478,0.781446540880503,0.783018867924528,0.784591194968553,
0.786163522012579,0.787735849056604,0.789308176100629,0.790880503144654,
0.792452830188679,0.794025157232704,0.79559748427673,0.797169811320755,
0.79874213836478,0.800314465408805,0.80188679245283,0.803459119496855,0.805031446540881,
0.806603773584906,0.808176100628931,0.809748427672956,0.811320754716981,
0.812893081761006,0.814465408805031,0.816037735849057,0.817610062893082,
0.819182389937107,0.820754716981132,0.822327044025157,0.823899371069182,
0.825471698113208,0.827044025157233,0.828616352201258,0.830188679245283,
0.831761006289308,0.833333333333333,0.834905660377358,0.836477987421384,
0.838050314465409,0.839622641509434,0.841194968553459,0.842767295597484,
0.844339622641509,0.845911949685535,0.84748427672956,0.849056603773585,
0.85062893081761,0.852201257861635,0.85377358490566,0.855345911949686,0.856918238993711,
0.858490566037736,0.860062893081761,0.861635220125786,0.863207547169811,
0.864779874213837,0.866352201257862,0.867924528301887,0.869496855345912,
0.871069182389937,0.872641509433962,0.874213836477987,0.875786163522013,
0.877358490566038,0.878930817610063,0.880503144654088,0.882075471698113,
0.883647798742138,0.885220125786163,0.886792452830189,0.888364779874214,
0.889937106918239,0.891509433962264,0.893081761006289,0.894654088050314,
0.89622641509434,0.897798742138365,0.89937106918239,0.900943396226415,0.90251572327044,
0.904088050314465,0.905660377358491,0.907232704402516,0.908805031446541,
0.910377358490566,0.911949685534591,0.913522012578616,0.915094339622642,
0.916666666666667,0.918238993710692,0.919811320754717,0.921383647798742,
0.922955974842767,0.924528301886792,0.926100628930818,0.927672955974843,
0.929245283018868,0.930817610062893,0.932389937106918,0.933962264150943,
0.935534591194969,0.937106918238994,0.938679245283019,0.940251572327044,
0.941823899371069,0.943396226415094,0.944968553459119,0.946540880503145,
0.94811320754717,0.949685534591195,0.95125786163522,0.952830188679245,0.95440251572327,
0.955974842767296,0.957547169811321,0.959119496855346,0.960691823899371,
0.962264150943396,0.963836477987421,0.965408805031447,0.966981132075472,
0.968553459119497,0.970125786163522,0.971698113207547,0.973270440251572,
0.974842767295597,0.976415094339623,0.977987421383648,0.979559748427673,
0.981132075471698,0.982704402515723,0.984276729559748,0.985849056603774,
0.987421383647799,0.988993710691824,0.990566037735849,0.992138364779874,
0.993710691823899,0.995283018867924,0.99685534591195,0.997310988253444),
 .UNSPECIFIED.)
GEOMETRIC_REPRESENTATION_ITEM()
RATIONAL_B_SPLINE_SURFACE(((1.,0.866025403784439,1.,0.866025403784439,1.,
0.866025403784439,1.,0.866025403784439,1.,0.866025403784439,1.,0.866025403784439,
1.,0.866025403784439,1.,0.866025403784439,1.,0.866025403784439,1.,0.866025403784439,
1.,0.866025403784439,1.,0.866025403784439,1.,0.866025403784439,1.,0.866025403784439,
1.,0.866025403784439,1.,0.866025403784439,1.,0.866025403784439,1.,0.866025403784439,
1.,0.866025403784439,1.,0.866025403784439,1.,0.866025403784439,1.,0.866025403784439,
1.,0.866025403784439,1.,0.866025403784439,1.,0.866025403784439,1.,0.866025403784439,
1.,0.866025403784439,1.,0.866025403784439,1.,0.866025403784439,1.,0.866025403784439,
1.,0.866025403784439,1.,0.866025403784439,1.,0.866025403784439,1.,0.866025403784439,
1.,0.866025403784439,1.,0.866025403784439,1.,0.866025403784439,1.,0.866025403784439,
1.,0.866025403784439,1.,0.866025403784439,1.,0.866025403784439,1.,0.866025403784439,
1.,0.866025403784439,1.,0.866025403784439,1.,0.866025403784439,1.,0.866025403784439,
1.,0.866025403784439,1.,0.866025403784439,1.,0.866025403784439,1.,0.866025403784439,
1.,0.866025403784439,1.,0.866025403784439,1.,0.866025403784439,1.,0.866025403784439,
1.,0.866025403784439,1.,0.866025403784439,1.,0.866025403784439,1.,0.866025403784439,
1.,0.866025403784439,1.,0.866025403784439,1.,0.866025403784439,1.,0.866025403784439,
1.,0.866025403784439,1.,0.866025403784439,1.,0.866025403784439,1.,0.866025403784439,
1.,0.866025403784439,1.,0.866025403784439,1.,0.866025403784439,1.,0.866025403784439,
1.,0.866025403784439,1.,0.866025403784439,1.,0.866025403784439,1.,0.866025403784439,
1.,0.866025403784439,1.,0.866025403784439,1.,0.866025403784439,1.,0.866025403784439,
1.,0.866025403784439,1.,0.866025403784439,1.,0.866025403784439,1.,0.866025403784439,
1.,0.866025403784439,1.,0.866025403784439,1.,0.866025403784439,1.,0.866025403784439,
1.,0.866025403784439,1.,0.866025403784439,1.,0.866025403784439,1.,0.866025403784439,
1.,0.866025403784439,1.,0.866025403784439,1.,0.866025403784439,1.,0.866025403784439,
1.,0.866025403784439,1.,0.866025403784439,1.,0.866025403784439,1.,0.866025403784439,
1.,0.866025403784439,1.,0.866025403784439,1.,0.866025403784439,1.,0.866025403784439,
1.,0.866025403784439,1.,0.866025403784439,1.,0.866025403784439,1.,0.866025403784439,
1.,0.866025403784439,1.,0.866025403784439,1.,0.866025403784439,1.,0.866025403784439,
1.,0.866025403784439,1.,0.866025403784439,1.,0.866025403784439,1.,0.866025403784439,
1.,0.866025403784439,1.,0.866025403784439,1.,0.866025403784439,1.,0.866025403784439,
1.,0.866025403784439,1.,0.866025403784439,1.,0.866025403784439,1.,0.866025403784439,
1.,0.866025403784439,1.,0.866025403784439,1.,0.866025403784439,1.,0.866025403784439,
1.,0.866025403784439,1.,0.866025403784439,1.,0.866025403784439,1.,0.866025403784439,
1.,0.866025403784439,1.,0.866025403784439,1.,0.866025403784439,1.,0.866025403784439,
1.,0.866025403784439,1.,0.866025403784439,1.,0.866025403784439,1.,0.866025403784439,
1.,0.866025403784439,1.,0.866025403784439,1.,0.866025403784439,1.,0.866025403784439,
1.,0.866025403784439,1.,0.866025403784439,1.,0.866025403784439,1.,0.866025403784439,
1.,0.866025403784439,1.,0.866025403784439,1.,0.866025403784439,1.,0.866025403784439,
1.,0.866025403784439,1.,0.866025403784439,1.,0.866025403784439,1.,0.866025403784439,
1.,0.866025403784439,1.,0.866025403784439,1.,0.866025403784439,1.,0.866025403784439,
1.,0.866025403784439,1.,0.866025403784439,1.,0.866025403784439,1.,0.866025403784439,
1.,0.866025403784439,1.,0.866025403784439,1.,0.866025403784439,1.,0.866025403784439,
1.,0.866025403784439,1.,0.866025403784439,1.,0.866025403784439,1.,0.866025403784439,
1.,0.866025403784439,1.,0.866025403784439,1.,0.866025403784439,1.,0.866025403784439,
1.,0.866025403784439,1.,0.866025403784439,1.,0.866025403784439,1.,0.866025403784439,
1.,0.866025403784439,1.,0.866025403784439,1.,0.866025403784439,1.,0.866025403784439,
1.,0.866025403784439,1.,0.866025403784439,1.,0.866025403784439,1.,0.866025403784439,
1.,0.866025403784439,1.,0.866025403784439,1.,0.866025403784439,1.,0.866025403784439,
1.,0.866025403784439,1.,0.866025403784439,1.,0.866025403784439,1.,0.866025403784439,
1.,0.866025403784439,1.,0.866025403784439,1.,0.866025403784439,1.,0.866025403784439,
1.,0.866025403784439,1.,0.866025403784439,1.,0.866025403784439,1.,0.866025403784439,
1.,0.866025403784439,1.,0.866025403784439,1.,0.866025403784439,1.,0.866025403784439,
1.,0.866025403784439,1.,0.866025403784439,1.,0.866025403784439,1.,0.866025403784439,
1.,0.866025403784439,1.,0.866025403784439,1.,0.866025403784439,1.,0.866025403784439,
1.,0.866025403784439,1.,0.866025403784439,1.,0.866025403784439,1.,0.866025403784439,
1.,0.866025403784439,1.,0.866025403784439,1.,0.866025403784439,1.,0.866025403784439,
1.,0.866025403784439,1.,0.866025403784439,1.,0.866025403784439,1.,0.866025403784439,
1.,0.866025403784439,1.,0.866025403784439,1.,0.866025403784439,1.,0.866025403784439,
1.,0.866025403784439,1.,0.866025403784439,1.,0.866025403784439,1.,0.866025403784439,
1.,0.866025403784439,1.,0.866025403784439,1.,0.866025403784439,1.,0.866025403784439,
1.,0.866025403784439,1.,0.866025403784439,1.,0.866025403784439,1.,0.866025403784439,
1.,0.866025403784439,1.,0.866025403784439,1.,0.866025403784439,1.,0.866025403784439,
1.,0.866025403784439,1.,0.866025403784439,1.,0.866025403784439,1.,0.866025403784439,
1.,0.866025403784439,1.,0.866025403784439,1.,0.866025403784439,1.,0.866025403784439,
1.,0.866025403784439,1.,0.866025403784439,1.,0.866025403784439,1.,0.866025403784439,
1.,0.866025403784439,1.,0.866025403784439,1.,0.866025403784439,1.,0.866025403784439,
1.,0.866025403784439,1.,0.866025403784439,1.,0.866025403784439,1.,0.866025403784439,
1.,0.866025403784439,1.,0.866025403784439,1.,0.866025403784439,1.,0.866025403784439,
1.,0.866025403784439,1.,0.866025403784439,1.,0.866025403784439,1.,0.866025403784439,
1.,0.866025403784439,1.,0.866025403784439,1.,0.866025403784439,1.,0.866025403784439,
1.,0.866025403784439,1.,0.866025403784439,1.,0.866025403784439,1.,0.866025403784439,
1.,0.866025403784439,1.,0.866025403784439,1.,0.866025403784439,1.,0.866025403784439,
1.,0.866025403784439,1.,0.866025403784439,1.,0.866025403784439,1.,0.866025403784439,
1.,0.866025403784439,1.,0.866025403784439,1.,0.866025403784439,1.,0.866025403784439,
1.,0.866025403784439,1.,0.866025403784439,1.,0.866025403784439,1.,0.866025403784439,
1.,0.866025403784439,1.,0.866025403784439,1.,0.866025403784439,1.,0.866025403784439,
1.,0.866025403784439,1.,0.866025403784439,1.,0.866025403784439,1.,0.866025403784439,
1.,0.866025403784439,1.,0.866025403784439,1.,0.866025403784439,1.,0.866025403784439,
1.,0.866025403784439,1.,0.866025403784439,1.,0.866025403784439,1.,0.866025403784439,
1.,0.866025403784439,1.,0.866025403784439,1.,0.866025403784439,1.,0.866025403784439,
1.,0.866025403784439,1.,0.866025403784439,1.,0.866025403784439,1.,0.866025403784439,
1.,0.866025403784439,1.,0.866025403784439,1.,0.866025403784439,1.,0.866025403784439,
1.,0.866025403784439,1.,0.866025403784439,1.,0.866025403784439,1.,0.866025403784439,
1.,0.866025403784439,1.,0.866025403784439,1.,0.866025403784439,1.,0.866025403784439,
1.,0.866025403784439,1.,0.866025403784439,1.,0.866025403784439,1.,0.866025403784439,
1.,0.866025403784439,1.,0.866025403784439,1.,0.866025403784439,1.,0.866025403784439,
1.,0.866025403784439,1.,0.866025403784439,1.,0.866025403784439,1.,0.866025403784439,
1.,0.866025403784439,1.,0.866025403784439,1.,0.866025403784439,1.,0.866025403784439,
1.,0.866025403784439,1.,0.866025403784439,1.,0.866025403784439,1.,0.866025403784439,
1.,0.866025403784439,1.,0.866025403784439,1.,0.866025403784439,1.,0.866025403784439,
1.,0.866025403784439,1.,0.866025403784439,1.,0.866025403784439,1.,0.866025403784439,
1.,0.866025403784439,1.,0.866025403784439,1.,0.866025403784439,1.,0.866025403784439,
1.,0.866025403784439,1.,0.866025403784439,1.,0.866025403784439,1.,0.866025403784439,
1.,0.866025403784439,1.,0.866025403784439,1.,0.866025403784439,1.,0.866025403784439,
1.,0.866025403784439,1.,0.866025403784439,1.,0.866025403784439,1.,0.866025403784439,
1.,0.866025403784439,1.,0.866025403784439,1.,0.866025403784439,1.,0.866025403784439,
1.,0.866025403784439,1.,0.866025403784439,1.,0.866025403784439,1.,0.866025403784439,
1.,0.866025403784439,1.,0.866025403784439,1.,0.866025403784439,1.,0.866025403784439,
1.,0.866025403784439,1.,0.866025403784439,1.,0.866025403784439,1.,0.866025403784439,
1.,0.866025403784439,1.,0.866025403784439,1.,0.866025403784439,1.,0.866025403784439,
1.,0.866025403784439,1.,0.866025403784439,1.,0.866025403784439,1.,0.866025403784439,
1.,0.866025403784439,1.,0.866025403784439,1.,0.866025403784439,1.,0.866025403784439,
1.,0.866025403784439,1.,0.866025403784439,1.,0.866025403784439,1.,0.866025403784439,
1.,0.866025403784439,1.,0.866025403784439,1.,0.866025403784439,1.,0.866025403784439,
1.,0.866025403784439,1.,0.866025403784439,1.,0.866025403784439,1.,0.866025403784439,
1.,0.866025403784439,1.,0.866025403784439,1.,0.866025403784439,1.,0.866025403784439,
1.,0.866025403784439,1.,0.866025403784439,1.,0.866025403784439,1.,0.866025403784439,
1.,0.866025403784439,1.,0.866025403784439,1.,0.866025403784439,1.,0.866025403784439,
1.,0.866025403784439,1.,0.866025403784439,1.,0.866025403784439,1.,0.866025403784439,
1.,0.866025403784439,1.,0.866025403784439,1.,0.866025403784439,1.,0.866025403784439,
1.,0.866025403784439,1.,0.866025403784439,1.,0.866025403784439,1.,0.866025403784439,
1.,0.866025403784439,1.,0.866025403784439,1.,0.866025403784439,1.,0.866025403784439,
1.,0.866025403784439,1.,0.866025403784439,1.,0.866025403784439,1.,0.866025403784439,
1.,0.866025403784439,1.,0.866025403784439,1.,0.866025403784439,1.,0.866025403784439,
1.,0.866025403784439,1.,0.866025403784439,1.,0.866025403784439,1.,0.866025403784439,
1.,0.866025403784439,1.,0.866025403784439,1.,0.866025403784439,1.,0.866025403784439,
1.,0.866025403784439,1.,0.866025403784439,1.,0.866025403784439,1.,0.866025403784439,
1.,0.866025403784439,1.,0.866025403784439,1.,0.866025403784439,1.,0.866025403784439,
1.,0.866025403784439,1.,0.866025403784439,1.,0.866025403784439,1.,0.866025403784439,
1.,0.866025403784439,1.,0.866025403784439,1.,0.866025403784439,1.,0.866025403784439,
1.,0.866025403784439,1.,0.866025403784439,1.,0.866025403784439,1.,0.866025403784439,
1.,0.866025403784439,1.,0.866025403784439,1.,0.866025403784439,1.,0.866025403784439,
1.,0.866025403784439,1.,0.866025403784439,1.,0.866025403784439,1.,0.866025403784439,
1.,0.866025403784439,1.,0.866025403784439,1.,0.866025403784439,1.,0.866025403784439,
1.,0.866025403784439,1.,0.866025403784439,1.,0.866025403784439,1.,0.866025403784439,
1.,0.866025403784439,1.,0.866025403784439,1.,0.866025403784439,1.,0.866025403784439,
1.,0.866025403784439,1.,0.866025403784439,1.,0.866025403784439,1.,0.866025403784439,
1.,0.866025403784439,1.,0.866025403784439,1.,0.866025403784439,1.,0.866025403784439,
1.,0.866025403784439,1.,0.866025403784439,1.,0.866025403784439,1.,0.866025403784439,
1.,0.866025403784439,1.,0.866025403784439,1.,0.866025403784439,1.,0.866025403784439,
1.,0.866025403784439,1.,0.866025403784439,1.,0.866025403784439,1.,0.866025403784439,
1.,0.866025403784439,1.,0.866025403784439,1.,0.866025403784439,1.,0.866025403784439,
1.,0.866025403784439,1.,0.866025403784439,1.,0.866025403784439,1.,0.866025403784439,
1.,0.866025403784439,1.,0.866025403784439,1.,0.866025403784439,1.,0.866025403784439,
1.,0.866025403784439,1.,0.866025403784439,1.,0.866025403784439,1.,0.866025403784439,
1.,0.866025403784439,1.,0.866025403784439,1.,0.866025403784439,1.,0.866025403784439,
1.,0.866025403784439,1.,0.866025403784439,1.,0.866025403784439,1.,0.866025403784439,
1.,0.866025403784439,1.,0.866025403784439,1.,0.866025403784439,1.,0.866025403784439,
1.,0.866025403784439,1.,0.866025403784439,1.,0.866025403784439,1.,0.866025403784439,
1.,0.866025403784439,1.,0.866025403784439,1.,0.866025403784439,1.,0.866025403784439,
1.,0.866025403784439,1.,0.866025403784439,1.,0.866025403784439,1.,0.866025403784439,
1.,0.866025403784439,1.,0.866025403784439,1.,0.866025403784439,1.,0.866025403784439,
1.,0.866025403784439,1.,0.866025403784439,1.,0.866025403784439,1.,0.866025403784439,
1.,0.866025403784439,1.,0.866025403784439,1.,0.866025403784439,1.,0.866025403784439,
1.,0.866025403784439,1.,0.866025403784439,1.,0.866025403784439,1.,0.866025403784439,
1.,0.866025403784439,1.,0.866025403784439,1.,0.866025403784439,1.,0.866025403784439,
1.,0.866025403784439,1.,0.866025403784439,1.,0.866025403784439,1.,0.866025403784439,
1.,0.866025403784439,1.,0.866025403784439,1.,0.866025403784439,1.,0.866025403784439,
1.,0.866025403784439,1.,0.866025403784439,1.,0.866025403784439,1.,0.866025403784439,
1.,0.866025403784439,1.,0.866025403784439,1.,0.866025403784439,1.,0.866025403784439,
1.,0.866025403784439,1.,0.866025403784439,1.,0.866025403784439,1.,0.866025403784439,
1.,0.866025403784439,1.,0.866025403784439,1.,0.866025403784439,1.,0.866025403784439,
1.,0.866025403784439,1.,0.866025403784439,1.,0.866025403784439,1.,0.866025403784439,
1.,0.866025403784439,1.,0.866025403784439,1.,0.866025403784439,1.,0.866025403784439,
1.,0.866025403784439,1.,0.866025403784439,1.,0.866025403784439,1.,0.866025403784439,
1.,0.866025403784439,1.,0.866025403784439,1.,0.866025403784439,1.,0.866025403784439,
1.,0.866025403784439,1.,0.866025403784439,1.,0.866025403784439,1.,0.866025403784439,
1.,0.866025403784439,1.,0.866025403784439,1.,0.866025403784439,1.,0.866025403784439,
1.,0.866025403784439,1.,0.866025403784439,1.,0.866025403784439,1.,0.866025403784439,
1.,0.961175698813797,0.944853071902794),(1.,0.866025403784439,1.,0.866025403784439,
1.,0.866025403784439,1.,0.866025403784439,1.,0.866025403784439,1.,0.866025403784439,
1.,0.866025403784439,1.,0.866025403784439,1.,0.866025403784439,1.,0.866025403784439,
1.,0.866025403784439,1.,0.866025403784439,1.,0.866025403784439,1.,0.866025403784439,
1.,0.866025403784439,1.,0.866025403784439,1.,0.866025403784439,1.,0.866025403784439,
1.,0.866025403784439,1.,0.866025403784439,1.,0.866025403784439,1.,0.866025403784439,
1.,0.866025403784439,1.,0.866025403784439,1.,0.866025403784439,1.,0.866025403784439,
1.,0.866025403784439,1.,0.866025403784439,1.,0.866025403784439,1.,0.866025403784439,
1.,0.866025403784439,1.,0.866025403784439,1.,0.866025403784439,1.,0.866025403784439,
1.,0.866025403784439,1.,0.866025403784439,1.,0.866025403784439,1.,0.866025403784439,
1.,0.866025403784439,1.,0.866025403784439,1.,0.866025403784439,1.,0.866025403784439,
1.,0.866025403784439,1.,0.866025403784439,1.,0.866025403784439,1.,0.866025403784439,
1.,0.866025403784439,1.,0.866025403784439,1.,0.866025403784439,1.,0.866025403784439,
1.,0.866025403784439,1.,0.866025403784439,1.,0.866025403784439,1.,0.866025403784439,
1.,0.866025403784439,1.,0.866025403784439,1.,0.866025403784439,1.,0.866025403784439,
1.,0.866025403784439,1.,0.866025403784439,1.,0.866025403784439,1.,0.866025403784439,
1.,0.866025403784439,1.,0.866025403784439,1.,0.866025403784439,1.,0.866025403784439,
1.,0.866025403784439,1.,0.866025403784439,1.,0.866025403784439,1.,0.866025403784439,
1.,0.866025403784439,1.,0.866025403784439,1.,0.866025403784439,1.,0.866025403784439,
1.,0.866025403784439,1.,0.866025403784439,1.,0.866025403784439,1.,0.866025403784439,
1.,0.866025403784439,1.,0.866025403784439,1.,0.866025403784439,1.,0.866025403784439,
1.,0.866025403784439,1.,0.866025403784439,1.,0.866025403784439,1.,0.866025403784439,
1.,0.866025403784439,1.,0.866025403784439,1.,0.866025403784439,1.,0.866025403784439,
1.,0.866025403784439,1.,0.866025403784439,1.,0.866025403784439,1.,0.866025403784439,
1.,0.866025403784439,1.,0.866025403784439,1.,0.866025403784439,1.,0.866025403784439,
1.,0.866025403784439,1.,0.866025403784439,1.,0.866025403784439,1.,0.866025403784439,
1.,0.866025403784439,1.,0.866025403784439,1.,0.866025403784439,1.,0.866025403784439,
1.,0.866025403784439,1.,0.866025403784439,1.,0.866025403784439,1.,0.866025403784439,
1.,0.866025403784439,1.,0.866025403784439,1.,0.866025403784439,1.,0.866025403784439,
1.,0.866025403784439,1.,0.866025403784439,1.,0.866025403784439,1.,0.866025403784439,
1.,0.866025403784439,1.,0.866025403784439,1.,0.866025403784439,1.,0.866025403784439,
1.,0.866025403784439,1.,0.866025403784439,1.,0.866025403784439,1.,0.866025403784439,
1.,0.866025403784439,1.,0.866025403784439,1.,0.866025403784439,1.,0.866025403784439,
1.,0.866025403784439,1.,0.866025403784439,1.,0.866025403784439,1.,0.866025403784439,
1.,0.866025403784439,1.,0.866025403784439,1.,0.866025403784439,1.,0.866025403784439,
1.,0.866025403784439,1.,0.866025403784439,1.,0.866025403784439,1.,0.866025403784439,
1.,0.866025403784439,1.,0.866025403784439,1.,0.866025403784439,1.,0.866025403784439,
1.,0.866025403784439,1.,0.866025403784439,1.,0.866025403784439,1.,0.866025403784439,
1.,0.866025403784439,1.,0.866025403784439,1.,0.866025403784439,1.,0.866025403784439,
1.,0.866025403784439,1.,0.866025403784439,1.,0.866025403784439,1.,0.866025403784439,
1.,0.866025403784439,1.,0.866025403784439,1.,0.866025403784439,1.,0.866025403784439,
1.,0.866025403784439,1.,0.866025403784439,1.,0.866025403784439,1.,0.866025403784439,
1.,0.866025403784439,1.,0.866025403784439,1.,0.866025403784439,1.,0.866025403784439,
1.,0.866025403784439,1.,0.866025403784439,1.,0.866025403784439,1.,0.866025403784439,
1.,0.866025403784439,1.,0.866025403784439,1.,0.866025403784439,1.,0.866025403784439,
1.,0.866025403784439,1.,0.866025403784439,1.,0.866025403784439,1.,0.866025403784439,
1.,0.866025403784439,1.,0.866025403784439,1.,0.866025403784439,1.,0.866025403784439,
1.,0.866025403784439,1.,0.866025403784439,1.,0.866025403784439,1.,0.866025403784439,
1.,0.866025403784439,1.,0.866025403784439,1.,0.866025403784439,1.,0.866025403784439,
1.,0.866025403784439,1.,0.866025403784439,1.,0.866025403784439,1.,0.866025403784439,
1.,0.866025403784439,1.,0.866025403784439,1.,0.866025403784439,1.,0.866025403784439,
1.,0.866025403784439,1.,0.866025403784439,1.,0.866025403784439,1.,0.866025403784439,
1.,0.866025403784439,1.,0.866025403784439,1.,0.866025403784439,1.,0.866025403784439,
1.,0.866025403784439,1.,0.866025403784439,1.,0.866025403784439,1.,0.866025403784439,
1.,0.866025403784439,1.,0.866025403784439,1.,0.866025403784439,1.,0.866025403784439,
1.,0.866025403784439,1.,0.866025403784439,1.,0.866025403784439,1.,0.866025403784439,
1.,0.866025403784439,1.,0.866025403784439,1.,0.866025403784439,1.,0.866025403784439,
1.,0.866025403784439,1.,0.866025403784439,1.,0.866025403784439,1.,0.866025403784439,
1.,0.866025403784439,1.,0.866025403784439,1.,0.866025403784439,1.,0.866025403784439,
1.,0.866025403784439,1.,0.866025403784439,1.,0.866025403784439,1.,0.866025403784439,
1.,0.866025403784439,1.,0.866025403784439,1.,0.866025403784439,1.,0.866025403784439,
1.,0.866025403784439,1.,0.866025403784439,1.,0.866025403784439,1.,0.866025403784439,
1.,0.866025403784439,1.,0.866025403784439,1.,0.866025403784439,1.,0.866025403784439,
1.,0.866025403784439,1.,0.866025403784439,1.,0.866025403784439,1.,0.866025403784439,
1.,0.866025403784439,1.,0.866025403784439,1.,0.866025403784439,1.,0.866025403784439,
1.,0.866025403784439,1.,0.866025403784439,1.,0.866025403784439,1.,0.866025403784439,
1.,0.866025403784439,1.,0.866025403784439,1.,0.866025403784439,1.,0.866025403784439,
1.,0.866025403784439,1.,0.866025403784439,1.,0.866025403784439,1.,0.866025403784439,
1.,0.866025403784439,1.,0.866025403784439,1.,0.866025403784439,1.,0.866025403784439,
1.,0.866025403784439,1.,0.866025403784439,1.,0.866025403784439,1.,0.866025403784439,
1.,0.866025403784439,1.,0.866025403784439,1.,0.866025403784439,1.,0.866025403784439,
1.,0.866025403784439,1.,0.866025403784439,1.,0.866025403784439,1.,0.866025403784439,
1.,0.866025403784439,1.,0.866025403784439,1.,0.866025403784439,1.,0.866025403784439,
1.,0.866025403784439,1.,0.866025403784439,1.,0.866025403784439,1.,0.866025403784439,
1.,0.866025403784439,1.,0.866025403784439,1.,0.866025403784439,1.,0.866025403784439,
1.,0.866025403784439,1.,0.866025403784439,1.,0.866025403784439,1.,0.866025403784439,
1.,0.866025403784439,1.,0.866025403784439,1.,0.866025403784439,1.,0.866025403784439,
1.,0.866025403784439,1.,0.866025403784439,1.,0.866025403784439,1.,0.866025403784439,
1.,0.866025403784439,1.,0.866025403784439,1.,0.866025403784439,1.,0.866025403784439,
1.,0.866025403784439,1.,0.866025403784439,1.,0.866025403784439,1.,0.866025403784439,
1.,0.866025403784439,1.,0.866025403784439,1.,0.866025403784439,1.,0.866025403784439,
1.,0.866025403784439,1.,0.866025403784439,1.,0.866025403784439,1.,0.866025403784439,
1.,0.866025403784439,1.,0.866025403784439,1.,0.866025403784439,1.,0.866025403784439,
1.,0.866025403784439,1.,0.866025403784439,1.,0.866025403784439,1.,0.866025403784439,
1.,0.866025403784439,1.,0.866025403784439,1.,0.866025403784439,1.,0.866025403784439,
1.,0.866025403784439,1.,0.866025403784439,1.,0.866025403784439,1.,0.866025403784439,
1.,0.866025403784439,1.,0.866025403784439,1.,0.866025403784439,1.,0.866025403784439,
1.,0.866025403784439,1.,0.866025403784439,1.,0.866025403784439,1.,0.866025403784439,
1.,0.866025403784439,1.,0.866025403784439,1.,0.866025403784439,1.,0.866025403784439,
1.,0.866025403784439,1.,0.866025403784439,1.,0.866025403784439,1.,0.866025403784439,
1.,0.866025403784439,1.,0.866025403784439,1.,0.866025403784439,1.,0.866025403784439,
1.,0.866025403784439,1.,0.866025403784439,1.,0.866025403784439,1.,0.866025403784439,
1.,0.866025403784439,1.,0.866025403784439,1.,0.866025403784439,1.,0.866025403784439,
1.,0.866025403784439,1.,0.866025403784439,1.,0.866025403784439,1.,0.866025403784439,
1.,0.866025403784439,1.,0.866025403784439,1.,0.866025403784439,1.,0.866025403784439,
1.,0.866025403784439,1.,0.866025403784439,1.,0.866025403784439,1.,0.866025403784439,
1.,0.866025403784439,1.,0.866025403784439,1.,0.866025403784439,1.,0.866025403784439,
1.,0.866025403784439,1.,0.866025403784439,1.,0.866025403784439,1.,0.866025403784439,
1.,0.866025403784439,1.,0.866025403784439,1.,0.866025403784439,1.,0.866025403784439,
1.,0.866025403784439,1.,0.866025403784439,1.,0.866025403784439,1.,0.866025403784439,
1.,0.866025403784439,1.,0.866025403784439,1.,0.866025403784439,1.,0.866025403784439,
1.,0.866025403784439,1.,0.866025403784439,1.,0.866025403784439,1.,0.866025403784439,
1.,0.866025403784439,1.,0.866025403784439,1.,0.866025403784439,1.,0.866025403784439,
1.,0.866025403784439,1.,0.866025403784439,1.,0.866025403784439,1.,0.866025403784439,
1.,0.866025403784439,1.,0.866025403784439,1.,0.866025403784439,1.,0.866025403784439,
1.,0.866025403784439,1.,0.866025403784439,1.,0.866025403784439,1.,0.866025403784439,
1.,0.866025403784439,1.,0.866025403784439,1.,0.866025403784439,1.,0.866025403784439,
1.,0.866025403784439,1.,0.866025403784439,1.,0.866025403784439,1.,0.866025403784439,
1.,0.866025403784439,1.,0.866025403784439,1.,0.866025403784439,1.,0.866025403784439,
1.,0.866025403784439,1.,0.866025403784439,1.,0.866025403784439,1.,0.866025403784439,
1.,0.866025403784439,1.,0.866025403784439,1.,0.866025403784439,1.,0.866025403784439,
1.,0.866025403784439,1.,0.866025403784439,1.,0.866025403784439,1.,0.866025403784439,
1.,0.866025403784439,1.,0.866025403784439,1.,0.866025403784439,1.,0.866025403784439,
1.,0.866025403784439,1.,0.866025403784439,1.,0.866025403784439,1.,0.866025403784439,
1.,0.866025403784439,1.,0.866025403784439,1.,0.866025403784439,1.,0.866025403784439,
1.,0.866025403784439,1.,0.866025403784439,1.,0.866025403784439,1.,0.866025403784439,
1.,0.866025403784439,1.,0.866025403784439,1.,0.866025403784439,1.,0.866025403784439,
1.,0.866025403784439,1.,0.866025403784439,1.,0.866025403784439,1.,0.866025403784439,
1.,0.866025403784439,1.,0.866025403784439,1.,0.866025403784439,1.,0.866025403784439,
1.,0.866025403784439,1.,0.866025403784439,1.,0.866025403784439,1.,0.866025403784439,
1.,0.866025403784439,1.,0.866025403784439,1.,0.866025403784439,1.,0.866025403784439,
1.,0.866025403784439,1.,0.866025403784439,1.,0.866025403784439,1.,0.866025403784439,
1.,0.866025403784439,1.,0.866025403784439,1.,0.866025403784439,1.,0.866025403784439,
1.,0.866025403784439,1.,0.866025403784439,1.,0.866025403784439,1.,0.866025403784439,
1.,0.866025403784439,1.,0.866025403784439,1.,0.866025403784439,1.,0.866025403784439,
1.,0.866025403784439,1.,0.866025403784439,1.,0.866025403784439,1.,0.866025403784439,
1.,0.866025403784439,1.,0.866025403784439,1.,0.866025403784439,1.,0.866025403784439,
1.,0.866025403784439,1.,0.866025403784439,1.,0.866025403784439,1.,0.866025403784439,
1.,0.866025403784439,1.,0.866025403784439,1.,0.866025403784439,1.,0.866025403784439,
1.,0.866025403784439,1.,0.866025403784439,1.,0.866025403784439,1.,0.866025403784439,
1.,0.866025403784439,1.,0.866025403784439,1.,0.866025403784439,1.,0.866025403784439,
1.,0.866025403784439,1.,0.866025403784439,1.,0.866025403784439,1.,0.866025403784439,
1.,0.866025403784439,1.,0.866025403784439,1.,0.866025403784439,1.,0.866025403784439,
1.,0.866025403784439,1.,0.866025403784439,1.,0.866025403784439,1.,0.866025403784439,
1.,0.866025403784439,1.,0.866025403784439,1.,0.866025403784439,1.,0.866025403784439,
1.,0.866025403784439,1.,0.866025403784439,1.,0.866025403784439,1.,0.866025403784439,
1.,0.866025403784439,1.,0.866025403784439,1.,0.866025403784439,1.,0.866025403784439,
1.,0.866025403784439,1.,0.866025403784439,1.,0.866025403784439,1.,0.866025403784439,
1.,0.866025403784439,1.,0.866025403784439,1.,0.866025403784439,1.,0.866025403784439,
1.,0.866025403784439,1.,0.866025403784439,1.,0.866025403784439,1.,0.866025403784439,
1.,0.866025403784439,1.,0.866025403784439,1.,0.866025403784439,1.,0.866025403784439,
1.,0.866025403784439,1.,0.866025403784439,1.,0.866025403784439,1.,0.866025403784439,
1.,0.866025403784439,1.,0.866025403784439,1.,0.866025403784439,1.,0.866025403784439,
1.,0.866025403784439,1.,0.866025403784439,1.,0.866025403784439,1.,0.866025403784439,
1.,0.866025403784439,1.,0.866025403784439,1.,0.866025403784439,1.,0.866025403784439,
1.,0.866025403784439,1.,0.866025403784439,1.,0.866025403784439,1.,0.866025403784439,
1.,0.866025403784439,1.,0.866025403784439,1.,0.866025403784439,1.,0.866025403784439,
1.,0.866025403784439,1.,0.866025403784439,1.,0.866025403784439,1.,0.866025403784439,
1.,0.866025403784439,1.,0.866025403784439,1.,0.866025403784439,1.,0.866025403784439,
1.,0.866025403784439,1.,0.866025403784439,1.,0.866025403784439,1.,0.866025403784439,
1.,0.866025403784439,1.,0.866025403784439,1.,0.866025403784439,1.,0.866025403784439,
1.,0.866025403784439,1.,0.866025403784439,1.,0.866025403784439,1.,0.866025403784439,
1.,0.866025403784439,1.,0.866025403784439,1.,0.866025403784439,1.,0.866025403784439,
1.,0.866025403784439,1.,0.866025403784439,1.,0.866025403784439,1.,0.866025403784439,
1.,0.866025403784439,1.,0.866025403784439,1.,0.866025403784439,1.,0.866025403784439,
1.,0.866025403784439,1.,0.866025403784439,1.,0.866025403784439,1.,0.866025403784439,
1.,0.866025403784439,1.,0.866025403784439,1.,0.866025403784439,1.,0.866025403784439,
1.,0.866025403784439,1.,0.866025403784439,1.,0.866025403784439,1.,0.866025403784439,
1.,0.866025403784439,1.,0.866025403784439,1.,0.866025403784439,1.,0.866025403784439,
1.,0.961175698813797,0.944853071902794)))
REPRESENTATION_ITEM('')
SURFACE()
);
#64=(
BOUNDED_SURFACE()
B_SPLINE_SURFACE(1,2,((#7227,#7228,#7229,#7230,#7231,#7232,#7233,#7234,
#7235,#7236,#7237,#7238,#7239,#7240,#7241,#7242,#7243,#7244,#7245,#7246,
#7247,#7248,#7249,#7250,#7251,#7252,#7253,#7254,#7255,#7256,#7257,#7258,
#7259,#7260,#7261,#7262,#7263,#7264,#7265,#7266,#7267,#7268,#7269,#7270,
#7271,#7272,#7273,#7274,#7275,#7276,#7277,#7278,#7279,#7280,#7281,#7282,
#7283,#7284,#7285,#7286,#7287,#7288,#7289,#7290,#7291,#7292,#7293,#7294,
#7295,#7296,#7297,#7298,#7299,#7300,#7301,#7302,#7303,#7304,#7305,#7306,
#7307,#7308,#7309,#7310,#7311,#7312,#7313,#7314,#7315,#7316,#7317,#7318,
#7319,#7320,#7321,#7322,#7323,#7324,#7325,#7326,#7327,#7328,#7329,#7330,
#7331,#7332,#7333,#7334,#7335,#7336,#7337,#7338,#7339,#7340,#7341,#7342,
#7343,#7344,#7345,#7346,#7347,#7348,#7349,#7350,#7351,#7352,#7353,#7354,
#7355,#7356,#7357,#7358,#7359,#7360,#7361,#7362,#7363,#7364,#7365,#7366,
#7367,#7368,#7369,#7370,#7371,#7372,#7373,#7374,#7375,#7376,#7377,#7378,
#7379,#7380,#7381,#7382,#7383,#7384,#7385,#7386,#7387,#7388,#7389,#7390,
#7391,#7392,#7393,#7394,#7395,#7396,#7397,#7398,#7399,#7400,#7401,#7402,
#7403,#7404,#7405,#7406,#7407,#7408,#7409,#7410,#7411,#7412,#7413,#7414,
#7415,#7416,#7417,#7418,#7419,#7420,#7421,#7422,#7423,#7424,#7425,#7426,
#7427,#7428,#7429,#7430,#7431,#7432,#7433,#7434,#7435,#7436,#7437,#7438,
#7439,#7440,#7441,#7442,#7443,#7444,#7445,#7446,#7447,#7448,#7449,#7450,
#7451,#7452,#7453,#7454,#7455,#7456,#7457,#7458,#7459,#7460,#7461,#7462,
#7463,#7464,#7465,#7466,#7467,#7468,#7469,#7470,#7471,#7472,#7473,#7474,
#7475,#7476,#7477,#7478,#7479,#7480,#7481,#7482,#7483,#7484,#7485,#7486,
#7487,#7488,#7489,#7490,#7491,#7492,#7493,#7494,#7495,#7496,#7497,#7498,
#7499,#7500,#7501,#7502,#7503,#7504,#7505,#7506,#7507,#7508,#7509,#7510,
#7511,#7512,#7513,#7514,#7515,#7516,#7517,#7518,#7519,#7520,#7521,#7522,
#7523,#7524,#7525,#7526,#7527,#7528,#7529,#7530,#7531,#7532,#7533,#7534,
#7535,#7536,#7537,#7538,#7539,#7540,#7541,#7542,#7543,#7544,#7545,#7546,
#7547,#7548,#7549,#7550,#7551,#7552,#7553,#7554,#7555,#7556,#7557,#7558,
#7559,#7560,#7561,#7562,#7563,#7564,#7565,#7566,#7567,#7568,#7569,#7570,
#7571,#7572,#7573,#7574,#7575,#7576,#7577,#7578,#7579,#7580,#7581,#7582,
#7583,#7584,#7585,#7586,#7587,#7588,#7589,#7590,#7591,#7592,#7593,#7594,
#7595,#7596,#7597,#7598,#7599,#7600,#7601,#7602,#7603,#7604,#7605,#7606,
#7607,#7608,#7609,#7610,#7611,#7612,#7613,#7614,#7615,#7616,#7617,#7618,
#7619,#7620,#7621,#7622,#7623,#7624,#7625,#7626,#7627,#7628,#7629,#7630,
#7631,#7632,#7633,#7634,#7635,#7636,#7637,#7638,#7639,#7640,#7641,#7642,
#7643,#7644,#7645,#7646,#7647,#7648,#7649,#7650,#7651,#7652,#7653,#7654,
#7655,#7656,#7657,#7658,#7659,#7660,#7661,#7662,#7663,#7664,#7665,#7666,
#7667,#7668,#7669,#7670,#7671,#7672,#7673,#7674,#7675,#7676,#7677,#7678,
#7679,#7680,#7681,#7682,#7683,#7684,#7685,#7686,#7687,#7688,#7689,#7690,
#7691,#7692,#7693,#7694,#7695,#7696,#7697,#7698,#7699,#7700,#7701,#7702,
#7703,#7704,#7705,#7706,#7707,#7708,#7709,#7710,#7711,#7712,#7713,#7714,
#7715,#7716,#7717,#7718,#7719,#7720,#7721,#7722,#7723,#7724,#7725,#7726,
#7727,#7728,#7729,#7730,#7731,#7732,#7733,#7734,#7735,#7736,#7737,#7738,
#7739,#7740,#7741,#7742,#7743,#7744,#7745,#7746,#7747,#7748,#7749,#7750,
#7751,#7752,#7753,#7754,#7755,#7756,#7757,#7758,#7759,#7760,#7761,#7762,
#7763,#7764,#7765,#7766,#7767,#7768,#7769,#7770,#7771,#7772,#7773,#7774,
#7775,#7776,#7777,#7778,#7779,#7780,#7781,#7782,#7783,#7784,#7785,#7786,
#7787,#7788,#7789,#7790,#7791,#7792,#7793,#7794,#7795,#7796,#7797,#7798,
#7799,#7800,#7801,#7802,#7803,#7804,#7805,#7806,#7807,#7808,#7809,#7810,
#7811,#7812,#7813,#7814,#7815,#7816,#7817,#7818,#7819,#7820,#7821,#7822,
#7823,#7824,#7825,#7826,#7827,#7828,#7829,#7830,#7831,#7832,#7833,#7834,
#7835,#7836,#7837,#7838,#7839,#7840,#7841,#7842,#7843,#7844,#7845,#7846,
#7847,#7848,#7849,#7850,#7851,#7852,#7853,#7854,#7855,#7856,#7857,#7858,
#7859,#7860,#7861,#7862,#7863,#7864,#7865,#7866,#7867,#7868,#7869,#7870,
#7871,#7872,#7873,#7874,#7875,#7876,#7877,#7878,#7879,#7880,#7881,#7882,
#7883,#7884,#7885,#7886,#7887,#7888,#7889,#7890,#7891,#7892,#7893,#7894,
#7895,#7896,#7897,#7898,#7899,#7900,#7901,#7902,#7903,#7904,#7905,#7906,
#7907,#7908,#7909,#7910,#7911,#7912,#7913,#7914,#7915,#7916,#7917,#7918,
#7919,#7920,#7921,#7922,#7923,#7924,#7925,#7926,#7927,#7928,#7929,#7930,
#7931,#7932,#7933,#7934,#7935,#7936,#7937,#7938,#7939,#7940,#7941,#7942,
#7943,#7944,#7945,#7946,#7947,#7948,#7949,#7950,#7951,#7952,#7953,#7954,
#7955,#7956,#7957,#7958,#7959,#7960,#7961,#7962,#7963,#7964,#7965,#7966,
#7967,#7968,#7969,#7970,#7971,#7972,#7973,#7974,#7975,#7976,#7977,#7978,
#7979,#7980,#7981,#7982,#7983,#7984,#7985,#7986,#7987,#7988,#7989,#7990,
#7991,#7992,#7993,#7994,#7995,#7996,#7997,#7998,#7999,#8000,#8001,#8002,
#8003,#8004,#8005,#8006,#8007,#8008,#8009,#8010,#8011,#8012,#8013,#8014,
#8015,#8016,#8017,#8018,#8019,#8020,#8021,#8022,#8023,#8024,#8025,#8026,
#8027,#8028,#8029,#8030,#8031,#8032,#8033,#8034,#8035,#8036,#8037,#8038,
#8039,#8040,#8041,#8042,#8043,#8044,#8045,#8046,#8047,#8048,#8049,#8050,
#8051,#8052,#8053,#8054,#8055,#8056,#8057,#8058,#8059,#8060,#8061,#8062,
#8063,#8064,#8065,#8066,#8067,#8068,#8069,#8070,#8071,#8072,#8073,#8074,
#8075,#8076,#8077,#8078,#8079,#8080,#8081,#8082,#8083,#8084,#8085,#8086,
#8087,#8088,#8089,#8090,#8091,#8092,#8093,#8094,#8095,#8096,#8097,#8098,
#8099,#8100,#8101,#8102,#8103,#8104,#8105,#8106,#8107,#8108,#8109,#8110,
#8111,#8112,#8113,#8114,#8115,#8116,#8117,#8118,#8119,#8120,#8121,#8122,
#8123,#8124,#8125,#8126,#8127,#8128,#8129,#8130,#8131,#8132,#8133,#8134,
#8135,#8136,#8137,#8138,#8139,#8140,#8141,#8142,#8143,#8144,#8145,#8146,
#8147,#8148,#8149,#8150,#8151,#8152,#8153,#8154,#8155,#8156,#8157,#8158,
#8159,#8160,#8161,#8162,#8163,#8164,#8165,#8166,#8167,#8168,#8169,#8170,
#8171,#8172,#8173,#8174,#8175,#8176,#8177,#8178,#8179,#8180,#8181,#8182,
#8183,#8184,#8185,#8186,#8187,#8188,#8189,#8190,#8191,#8192,#8193,#8194,
#8195,#8196,#8197,#8198,#8199,#8200,#8201,#8202,#8203,#8204,#8205,#8206,
#8207,#8208,#8209,#8210,#8211,#8212,#8213,#8214,#8215,#8216,#8217,#8218,
#8219,#8220,#8221,#8222,#8223,#8224,#8225,#8226,#8227,#8228,#8229,#8230,
#8231,#8232,#8233,#8234,#8235,#8236,#8237,#8238,#8239,#8240,#8241,#8242,
#8243,#8244,#8245,#8246,#8247,#8248,#8249,#8250,#8251,#8252,#8253,#8254,
#8255,#8256,#8257,#8258,#8259,#8260,#8261,#8262,#8263,#8264,#8265,#8266,
#8267,#8268,#8269,#8270,#8271,#8272,#8273,#8274,#8275,#8276,#8277,#8278,
#8279,#8280,#8281,#8282,#8283,#8284,#8285,#8286,#8287,#8288,#8289,#8290,
#8291,#8292,#8293,#8294,#8295,#8296,#8297,#8298,#8299,#8300,#8301,#8302,
#8303,#8304,#8305,#8306,#8307,#8308,#8309,#8310,#8311,#8312,#8313,#8314,
#8315,#8316,#8317,#8318,#8319,#8320,#8321,#8322,#8323,#8324,#8325,#8326,
#8327,#8328,#8329,#8330,#8331,#8332,#8333,#8334,#8335,#8336,#8337,#8338,
#8339,#8340,#8341,#8342,#8343,#8344,#8345,#8346,#8347,#8348,#8349,#8350,
#8351,#8352,#8353,#8354,#8355,#8356,#8357,#8358,#8359,#8360,#8361,#8362,
#8363,#8364,#8365,#8366,#8367,#8368,#8369,#8370,#8371,#8372,#8373,#8374,
#8375,#8376,#8377,#8378,#8379,#8380,#8381,#8382,#8383,#8384,#8385,#8386,
#8387,#8388,#8389,#8390,#8391,#8392,#8393,#8394,#8395,#8396,#8397,#8398,
#8399,#8400,#8401,#8402,#8403,#8404,#8405,#8406,#8407,#8408,#8409,#8410,
#8411,#8412,#8413,#8414,#8415,#8416,#8417,#8418,#8419,#8420,#8421,#8422,
#8423,#8424,#8425,#8426,#8427,#8428,#8429,#8430,#8431,#8432,#8433,#8434,
#8435,#8436,#8437,#8438,#8439,#8440,#8441,#8442,#8443,#8444,#8445,#8446,
#8447,#8448,#8449,#8450,#8451,#8452,#8453,#8454,#8455,#8456,#8457,#8458,
#8459,#8460,#8461,#8462,#8463,#8464,#8465,#8466,#8467,#8468,#8469,#8470,
#8471,#8472,#8473,#8474,#8475,#8476,#8477,#8478,#8479,#8480,#8481,#8482,
#8483,#8484,#8485,#8486,#8487,#8488,#8489,#8490,#8491,#8492,#8493,#8494,
#8495,#8496,#8497),(#8498,#8499,#8500,#8501,#8502,#8503,#8504,#8505,#8506,
#8507,#8508,#8509,#8510,#8511,#8512,#8513,#8514,#8515,#8516,#8517,#8518,
#8519,#8520,#8521,#8522,#8523,#8524,#8525,#8526,#8527,#8528,#8529,#8530,
#8531,#8532,#8533,#8534,#8535,#8536,#8537,#8538,#8539,#8540,#8541,#8542,
#8543,#8544,#8545,#8546,#8547,#8548,#8549,#8550,#8551,#8552,#8553,#8554,
#8555,#8556,#8557,#8558,#8559,#8560,#8561,#8562,#8563,#8564,#8565,#8566,
#8567,#8568,#8569,#8570,#8571,#8572,#8573,#8574,#8575,#8576,#8577,#8578,
#8579,#8580,#8581,#8582,#8583,#8584,#8585,#8586,#8587,#8588,#8589,#8590,
#8591,#8592,#8593,#8594,#8595,#8596,#8597,#8598,#8599,#8600,#8601,#8602,
#8603,#8604,#8605,#8606,#8607,#8608,#8609,#8610,#8611,#8612,#8613,#8614,
#8615,#8616,#8617,#8618,#8619,#8620,#8621,#8622,#8623,#8624,#8625,#8626,
#8627,#8628,#8629,#8630,#8631,#8632,#8633,#8634,#8635,#8636,#8637,#8638,
#8639,#8640,#8641,#8642,#8643,#8644,#8645,#8646,#8647,#8648,#8649,#8650,
#8651,#8652,#8653,#8654,#8655,#8656,#8657,#8658,#8659,#8660,#8661,#8662,
#8663,#8664,#8665,#8666,#8667,#8668,#8669,#8670,#8671,#8672,#8673,#8674,
#8675,#8676,#8677,#8678,#8679,#8680,#8681,#8682,#8683,#8684,#8685,#8686,
#8687,#8688,#8689,#8690,#8691,#8692,#8693,#8694,#8695,#8696,#8697,#8698,
#8699,#8700,#8701,#8702,#8703,#8704,#8705,#8706,#8707,#8708,#8709,#8710,
#8711,#8712,#8713,#8714,#8715,#8716,#8717,#8718,#8719,#8720,#8721,#8722,
#8723,#8724,#8725,#8726,#8727,#8728,#8729,#8730,#8731,#8732,#8733,#8734,
#8735,#8736,#8737,#8738,#8739,#8740,#8741,#8742,#8743,#8744,#8745,#8746,
#8747,#8748,#8749,#8750,#8751,#8752,#8753,#8754,#8755,#8756,#8757,#8758,
#8759,#8760,#8761,#8762,#8763,#8764,#8765,#8766,#8767,#8768,#8769,#8770,
#8771,#8772,#8773,#8774,#8775,#8776,#8777,#8778,#8779,#8780,#8781,#8782,
#8783,#8784,#8785,#8786,#8787,#8788,#8789,#8790,#8791,#8792,#8793,#8794,
#8795,#8796,#8797,#8798,#8799,#8800,#8801,#8802,#8803,#8804,#8805,#8806,
#8807,#8808,#8809,#8810,#8811,#8812,#8813,#8814,#8815,#8816,#8817,#8818,
#8819,#8820,#8821,#8822,#8823,#8824,#8825,#8826,#8827,#8828,#8829,#8830,
#8831,#8832,#8833,#8834,#8835,#8836,#8837,#8838,#8839,#8840,#8841,#8842,
#8843,#8844,#8845,#8846,#8847,#8848,#8849,#8850,#8851,#8852,#8853,#8854,
#8855,#8856,#8857,#8858,#8859,#8860,#8861,#8862,#8863,#8864,#8865,#8866,
#8867,#8868,#8869,#8870,#8871,#8872,#8873,#8874,#8875,#8876,#8877,#8878,
#8879,#8880,#8881,#8882,#8883,#8884,#8885,#8886,#8887,#8888,#8889,#8890,
#8891,#8892,#8893,#8894,#8895,#8896,#8897,#8898,#8899,#8900,#8901,#8902,
#8903,#8904,#8905,#8906,#8907,#8908,#8909,#8910,#8911,#8912,#8913,#8914,
#8915,#8916,#8917,#8918,#8919,#8920,#8921,#8922,#8923,#8924,#8925,#8926,
#8927,#8928,#8929,#8930,#8931,#8932,#8933,#8934,#8935,#8936,#8937,#8938,
#8939,#8940,#8941,#8942,#8943,#8944,#8945,#8946,#8947,#8948,#8949,#8950,
#8951,#8952,#8953,#8954,#8955,#8956,#8957,#8958,#8959,#8960,#8961,#8962,
#8963,#8964,#8965,#8966,#8967,#8968,#8969,#8970,#8971,#8972,#8973,#8974,
#8975,#8976,#8977,#8978,#8979,#8980,#8981,#8982,#8983,#8984,#8985,#8986,
#8987,#8988,#8989,#8990,#8991,#8992,#8993,#8994,#8995,#8996,#8997,#8998,
#8999,#9000,#9001,#9002,#9003,#9004,#9005,#9006,#9007,#9008,#9009,#9010,
#9011,#9012,#9013,#9014,#9015,#9016,#9017,#9018,#9019,#9020,#9021,#9022,
#9023,#9024,#9025,#9026,#9027,#9028,#9029,#9030,#9031,#9032,#9033,#9034,
#9035,#9036,#9037,#9038,#9039,#9040,#9041,#9042,#9043,#9044,#9045,#9046,
#9047,#9048,#9049,#9050,#9051,#9052,#9053,#9054,#9055,#9056,#9057,#9058,
#9059,#9060,#9061,#9062,#9063,#9064,#9065,#9066,#9067,#9068,#9069,#9070,
#9071,#9072,#9073,#9074,#9075,#9076,#9077,#9078,#9079,#9080,#9081,#9082,
#9083,#9084,#9085,#9086,#9087,#9088,#9089,#9090,#9091,#9092,#9093,#9094,
#9095,#9096,#9097,#9098,#9099,#9100,#9101,#9102,#9103,#9104,#9105,#9106,
#9107,#9108,#9109,#9110,#9111,#9112,#9113,#9114,#9115,#9116,#9117,#9118,
#9119,#9120,#9121,#9122,#9123,#9124,#9125,#9126,#9127,#9128,#9129,#9130,
#9131,#9132,#9133,#9134,#9135,#9136,#9137,#9138,#9139,#9140,#9141,#9142,
#9143,#9144,#9145,#9146,#9147,#9148,#9149,#9150,#9151,#9152,#9153,#9154,
#9155,#9156,#9157,#9158,#9159,#9160,#9161,#9162,#9163,#9164,#9165,#9166,
#9167,#9168,#9169,#9170,#9171,#9172,#9173,#9174,#9175,#9176,#9177,#9178,
#9179,#9180,#9181,#9182,#9183,#9184,#9185,#9186,#9187,#9188,#9189,#9190,
#9191,#9192,#9193,#9194,#9195,#9196,#9197,#9198,#9199,#9200,#9201,#9202,
#9203,#9204,#9205,#9206,#9207,#9208,#9209,#9210,#9211,#9212,#9213,#9214,
#9215,#9216,#9217,#9218,#9219,#9220,#9221,#9222,#9223,#9224,#9225,#9226,
#9227,#9228,#9229,#9230,#9231,#9232,#9233,#9234,#9235,#9236,#9237,#9238,
#9239,#9240,#9241,#9242,#9243,#9244,#9245,#9246,#9247,#9248,#9249,#9250,
#9251,#9252,#9253,#9254,#9255,#9256,#9257,#9258,#9259,#9260,#9261,#9262,
#9263,#9264,#9265,#9266,#9267,#9268,#9269,#9270,#9271,#9272,#9273,#9274,
#9275,#9276,#9277,#9278,#9279,#9280,#9281,#9282,#9283,#9284,#9285,#9286,
#9287,#9288,#9289,#9290,#9291,#9292,#9293,#9294,#9295,#9296,#9297,#9298,
#9299,#9300,#9301,#9302,#9303,#9304,#9305,#9306,#9307,#9308,#9309,#9310,
#9311,#9312,#9313,#9314,#9315,#9316,#9317,#9318,#9319,#9320,#9321,#9322,
#9323,#9324,#9325,#9326,#9327,#9328,#9329,#9330,#9331,#9332,#9333,#9334,
#9335,#9336,#9337,#9338,#9339,#9340,#9341,#9342,#9343,#9344,#9345,#9346,
#9347,#9348,#9349,#9350,#9351,#9352,#9353,#9354,#9355,#9356,#9357,#9358,
#9359,#9360,#9361,#9362,#9363,#9364,#9365,#9366,#9367,#9368,#9369,#9370,
#9371,#9372,#9373,#9374,#9375,#9376,#9377,#9378,#9379,#9380,#9381,#9382,
#9383,#9384,#9385,#9386,#9387,#9388,#9389,#9390,#9391,#9392,#9393,#9394,
#9395,#9396,#9397,#9398,#9399,#9400,#9401,#9402,#9403,#9404,#9405,#9406,
#9407,#9408,#9409,#9410,#9411,#9412,#9413,#9414,#9415,#9416,#9417,#9418,
#9419,#9420,#9421,#9422,#9423,#9424,#9425,#9426,#9427,#9428,#9429,#9430,
#9431,#9432,#9433,#9434,#9435,#9436,#9437,#9438,#9439,#9440,#9441,#9442,
#9443,#9444,#9445,#9446,#9447,#9448,#9449,#9450,#9451,#9452,#9453,#9454,
#9455,#9456,#9457,#9458,#9459,#9460,#9461,#9462,#9463,#9464,#9465,#9466,
#9467,#9468,#9469,#9470,#9471,#9472,#9473,#9474,#9475,#9476,#9477,#9478,
#9479,#9480,#9481,#9482,#9483,#9484,#9485,#9486,#9487,#9488,#9489,#9490,
#9491,#9492,#9493,#9494,#9495,#9496,#9497,#9498,#9499,#9500,#9501,#9502,
#9503,#9504,#9505,#9506,#9507,#9508,#9509,#9510,#9511,#9512,#9513,#9514,
#9515,#9516,#9517,#9518,#9519,#9520,#9521,#9522,#9523,#9524,#9525,#9526,
#9527,#9528,#9529,#9530,#9531,#9532,#9533,#9534,#9535,#9536,#9537,#9538,
#9539,#9540,#9541,#9542,#9543,#9544,#9545,#9546,#9547,#9548,#9549,#9550,
#9551,#9552,#9553,#9554,#9555,#9556,#9557,#9558,#9559,#9560,#9561,#9562,
#9563,#9564,#9565,#9566,#9567,#9568,#9569,#9570,#9571,#9572,#9573,#9574,
#9575,#9576,#9577,#9578,#9579,#9580,#9581,#9582,#9583,#9584,#9585,#9586,
#9587,#9588,#9589,#9590,#9591,#9592,#9593,#9594,#9595,#9596,#9597,#9598,
#9599,#9600,#9601,#9602,#9603,#9604,#9605,#9606,#9607,#9608,#9609,#9610,
#9611,#9612,#9613,#9614,#9615,#9616,#9617,#9618,#9619,#9620,#9621,#9622,
#9623,#9624,#9625,#9626,#9627,#9628,#9629,#9630,#9631,#9632,#9633,#9634,
#9635,#9636,#9637,#9638,#9639,#9640,#9641,#9642,#9643,#9644,#9645,#9646,
#9647,#9648,#9649,#9650,#9651,#9652,#9653,#9654,#9655,#9656,#9657,#9658,
#9659,#9660,#9661,#9662,#9663,#9664,#9665,#9666,#9667,#9668,#9669,#9670,
#9671,#9672,#9673,#9674,#9675,#9676,#9677,#9678,#9679,#9680,#9681,#9682,
#9683,#9684,#9685,#9686,#9687,#9688,#9689,#9690,#9691,#9692,#9693,#9694,
#9695,#9696,#9697,#9698,#9699,#9700,#9701,#9702,#9703,#9704,#9705,#9706,
#9707,#9708,#9709,#9710,#9711,#9712,#9713,#9714,#9715,#9716,#9717,#9718,
#9719,#9720,#9721,#9722,#9723,#9724,#9725,#9726,#9727,#9728,#9729,#9730,
#9731,#9732,#9733,#9734,#9735,#9736,#9737,#9738,#9739,#9740,#9741,#9742,
#9743,#9744,#9745,#9746,#9747,#9748,#9749,#9750,#9751,#9752,#9753,#9754,
#9755,#9756,#9757,#9758,#9759,#9760,#9761,#9762,#9763,#9764,#9765,#9766,
#9767,#9768)),.UNSPECIFIED.,.F.,.F.,.F.)
B_SPLINE_SURFACE_WITH_KNOTS((2,2),(3,2,2,2,2,2,2,2,2,2,2,2,2,2,2,2,2,2,
2,2,2,2,2,2,2,2,2,2,2,2,2,2,2,2,2,2,2,2,2,2,2,2,2,2,2,2,2,2,2,2,2,2,2,2,
2,2,2,2,2,2,2,2,2,2,2,2,2,2,2,2,2,2,2,2,2,2,2,2,2,2,2,2,2,2,2,2,2,2,2,2,
2,2,2,2,2,2,2,2,2,2,2,2,2,2,2,2,2,2,2,2,2,2,2,2,2,2,2,2,2,2,2,2,2,2,2,2,
2,2,2,2,2,2,2,2,2,2,2,2,2,2,2,2,2,2,2,2,2,2,2,2,2,2,2,2,2,2,2,2,2,2,2,2,
2,2,2,2,2,2,2,2,2,2,2,2,2,2,2,2,2,2,2,2,2,2,2,2,2,2,2,2,2,2,2,2,2,2,2,2,
2,2,2,2,2,2,2,2,2,2,2,2,2,2,2,2,2,2,2,2,2,2,2,2,2,2,2,2,2,2,2,2,2,2,2,2,
2,2,2,2,2,2,2,2,2,2,2,2,2,2,2,2,2,2,2,2,2,2,2,2,2,2,2,2,2,2,2,2,2,2,2,2,
2,2,2,2,2,2,2,2,2,2,2,2,2,2,2,2,2,2,2,2,2,2,2,2,2,2,2,2,2,2,2,2,2,2,2,2,
2,2,2,2,2,2,2,2,2,2,2,2,2,2,2,2,2,2,2,2,2,2,2,2,2,2,2,2,2,2,2,2,2,2,2,2,
2,2,2,2,2,2,2,2,2,2,2,2,2,2,2,2,2,2,2,2,2,2,2,2,2,2,2,2,2,2,2,2,2,2,2,2,
2,2,2,2,2,2,2,2,2,2,2,2,2,2,2,2,2,2,2,2,2,2,2,2,2,2,2,2,2,2,2,2,2,2,2,2,
2,2,2,2,2,2,2,2,2,2,2,2,2,2,2,2,2,2,2,2,2,2,2,2,2,2,2,2,2,2,2,2,2,2,2,2,
2,2,2,2,2,2,2,2,2,2,2,2,2,2,2,2,2,2,2,2,2,2,2,2,2,2,2,2,2,2,2,2,2,2,2,2,
2,2,2,2,2,2,2,2,2,2,2,2,2,2,2,2,2,2,2,2,2,2,2,2,2,2,2,2,2,2,2,2,2,2,2,2,
2,2,2,2,2,2,2,2,2,2,2,2,2,2,2,2,2,2,2,2,2,2,2,2,2,2,2,2,2,2,2,2,2,2,2,2,
2,2,2,2,2,2,2,2,2,2,2,2,2,2,2,2,2,2,2,2,2,2,2,2,2,2,2,2,2,2,2,2,2,2,2,2,
2,2,2,2,2,2,2,2,2,2,2,2,2,2,2,2,2,2,2,2,2,2,2,2,2,2,2,2,2,2,2,2,2,2,2,2,
2,2,2,2,2,3),(-0.0161647051742108,1.),(0.,0.00157232704402516,0.00314465408805031,
0.00471698113207547,0.00628930817610063,0.00786163522012579,0.00943396226415094,
0.0110062893081761,0.0125786163522013,0.0141509433962264,0.0157232704402516,
0.0172955974842767,0.0188679245283019,0.020440251572327,0.0220125786163522,
0.0235849056603774,0.0251572327044025,0.0267295597484277,0.0283018867924528,
0.029874213836478,0.0314465408805031,0.0330188679245283,0.0345911949685535,
0.0361635220125786,0.0377358490566038,0.0393081761006289,0.0408805031446541,
0.0424528301886792,0.0440251572327044,0.0455974842767296,0.0471698113207547,
0.0487421383647799,0.050314465408805,0.0518867924528302,0.0534591194968553,
0.0550314465408805,0.0566037735849057,0.0581761006289308,0.059748427672956,
0.0613207547169811,0.0628930817610063,0.0644654088050314,0.0660377358490566,
0.0676100628930818,0.0691823899371069,0.0707547169811321,0.0723270440251572,
0.0738993710691824,0.0754716981132075,0.0770440251572327,0.0786163522012579,
0.080188679245283,0.0817610062893082,0.0833333333333333,0.0849056603773585,
0.0864779874213836,0.0880503144654088,0.089622641509434,0.0911949685534591,
0.0927672955974843,0.0943396226415094,0.0959119496855346,0.0974842767295598,
0.0990566037735849,0.10062893081761,0.102201257861635,0.10377358490566,
0.105345911949686,0.106918238993711,0.108490566037736,0.110062893081761,
0.111635220125786,0.113207547169811,0.114779874213836,0.116352201257862,
0.117924528301887,0.119496855345912,0.121069182389937,0.122641509433962,
0.124213836477987,0.125786163522013,0.127358490566038,0.128930817610063,
0.130503144654088,0.132075471698113,0.133647798742138,0.135220125786164,
0.136792452830189,0.138364779874214,0.139937106918239,0.141509433962264,
0.143081761006289,0.144654088050314,0.14622641509434,0.147798742138365,
0.14937106918239,0.150943396226415,0.15251572327044,0.154088050314465,0.155660377358491,
0.157232704402516,0.158805031446541,0.160377358490566,0.161949685534591,
0.163522012578616,0.165094339622642,0.166666666666667,0.168238993710692,
0.169811320754717,0.171383647798742,0.172955974842767,0.174528301886792,
0.176100628930818,0.177672955974843,0.179245283018868,0.180817610062893,
0.182389937106918,0.183962264150943,0.185534591194969,0.187106918238994,
0.188679245283019,0.190251572327044,0.191823899371069,0.193396226415094,
0.19496855345912,0.196540880503145,0.19811320754717,0.199685534591195,0.20125786163522,
0.202830188679245,0.20440251572327,0.205974842767296,0.207547169811321,
0.209119496855346,0.210691823899371,0.212264150943396,0.213836477987421,
0.215408805031447,0.216981132075472,0.218553459119497,0.220125786163522,
0.221698113207547,0.223270440251572,0.224842767295597,0.226415094339623,
0.227987421383648,0.229559748427673,0.231132075471698,0.232704402515723,
0.234276729559748,0.235849056603774,0.237421383647799,0.238993710691824,
0.240566037735849,0.242138364779874,0.243710691823899,0.245283018867925,
0.24685534591195,0.248427672955975,0.25,0.251572327044025,0.25314465408805,
0.254716981132075,0.256289308176101,0.257861635220126,0.259433962264151,
0.261006289308176,0.262578616352201,0.264150943396226,0.265723270440252,
0.267295597484277,0.268867924528302,0.270440251572327,0.272012578616352,
0.273584905660377,0.275157232704403,0.276729559748428,0.278301886792453,
0.279874213836478,0.281446540880503,0.283018867924528,0.284591194968553,
0.286163522012579,0.287735849056604,0.289308176100629,0.290880503144654,
0.292452830188679,0.294025157232704,0.29559748427673,0.297169811320755,
0.29874213836478,0.300314465408805,0.30188679245283,0.303459119496855,0.30503144654088,
0.306603773584906,0.308176100628931,0.309748427672956,0.311320754716981,
0.312893081761006,0.314465408805031,0.316037735849057,0.317610062893082,
0.319182389937107,0.320754716981132,0.322327044025157,0.323899371069182,
0.325471698113208,0.327044025157233,0.328616352201258,0.330188679245283,
0.331761006289308,0.333333333333333,0.334905660377358,0.336477987421384,
0.338050314465409,0.339622641509434,0.341194968553459,0.342767295597484,
0.344339622641509,0.345911949685535,0.34748427672956,0.349056603773585,
0.35062893081761,0.352201257861635,0.35377358490566,0.355345911949686,0.356918238993711,
0.358490566037736,0.360062893081761,0.361635220125786,0.363207547169811,
0.364779874213836,0.366352201257862,0.367924528301887,0.369496855345912,
0.371069182389937,0.372641509433962,0.374213836477987,0.375786163522013,
0.377358490566038,0.378930817610063,0.380503144654088,0.382075471698113,
0.383647798742138,0.385220125786164,0.386792452830189,0.388364779874214,
0.389937106918239,0.391509433962264,0.393081761006289,0.394654088050314,
0.39622641509434,0.397798742138365,0.39937106918239,0.400943396226415,0.40251572327044,
0.404088050314465,0.405660377358491,0.407232704402516,0.408805031446541,
0.410377358490566,0.411949685534591,0.413522012578616,0.415094339622642,
0.416666666666667,0.418238993710692,0.419811320754717,0.421383647798742,
0.422955974842767,0.424528301886792,0.426100628930818,0.427672955974843,
0.429245283018868,0.430817610062893,0.432389937106918,0.433962264150943,
0.435534591194969,0.437106918238994,0.438679245283019,0.440251572327044,
0.441823899371069,0.443396226415094,0.44496855345912,0.446540880503145,
0.44811320754717,0.449685534591195,0.45125786163522,0.452830188679245,0.45440251572327,
0.455974842767296,0.457547169811321,0.459119496855346,0.460691823899371,
0.462264150943396,0.463836477987421,0.465408805031447,0.466981132075472,
0.468553459119497,0.470125786163522,0.471698113207547,0.473270440251572,
0.474842767295597,0.476415094339623,0.477987421383648,0.479559748427673,
0.481132075471698,0.482704402515723,0.484276729559748,0.485849056603774,
0.487421383647799,0.488993710691824,0.490566037735849,0.492138364779874,
0.493710691823899,0.495283018867925,0.49685534591195,0.498427672955975,
0.5,0.501572327044025,0.50314465408805,0.504716981132076,0.506289308176101,
0.507861635220126,0.509433962264151,0.511006289308176,0.512578616352201,
0.514150943396226,0.515723270440252,0.517295597484277,0.518867924528302,
0.520440251572327,0.522012578616352,0.523584905660377,0.525157232704403,
0.526729559748428,0.528301886792453,0.529874213836478,0.531446540880503,
0.533018867924528,0.534591194968553,0.536163522012579,0.537735849056604,
0.539308176100629,0.540880503144654,0.542452830188679,0.544025157232704,
0.54559748427673,0.547169811320755,0.54874213836478,0.550314465408805,0.55188679245283,
0.553459119496855,0.555031446540881,0.556603773584906,0.558176100628931,
0.559748427672956,0.561320754716981,0.562893081761006,0.564465408805031,
0.566037735849057,0.567610062893082,0.569182389937107,0.570754716981132,
0.572327044025157,0.573899371069182,0.575471698113208,0.577044025157233,
0.578616352201258,0.580188679245283,0.581761006289308,0.583333333333333,
0.584905660377358,0.586477987421384,0.588050314465409,0.589622641509434,
0.591194968553459,0.592767295597484,0.594339622641509,0.595911949685535,
0.59748427672956,0.599056603773585,0.60062893081761,0.602201257861635,0.60377358490566,
0.605345911949686,0.606918238993711,0.608490566037736,0.610062893081761,
0.611635220125786,0.613207547169811,0.614779874213837,0.616352201257862,
0.617924528301887,0.619496855345912,0.621069182389937,0.622641509433962,
0.624213836477987,0.625786163522013,0.627358490566038,0.628930817610063,
0.630503144654088,0.632075471698113,0.633647798742138,0.635220125786163,
0.636792452830189,0.638364779874214,0.639937106918239,0.641509433962264,
0.643081761006289,0.644654088050314,0.64622641509434,0.647798742138365,
0.64937106918239,0.650943396226415,0.65251572327044,0.654088050314465,0.655660377358491,
0.657232704402516,0.658805031446541,0.660377358490566,0.661949685534591,
0.663522012578616,0.665094339622642,0.666666666666667,0.668238993710692,
0.669811320754717,0.671383647798742,0.672955974842767,0.674528301886792,
0.676100628930818,0.677672955974843,0.679245283018868,0.680817610062893,
0.682389937106918,0.683962264150943,0.685534591194969,0.687106918238994,
0.688679245283019,0.690251572327044,0.691823899371069,0.693396226415094,
0.694968553459119,0.696540880503145,0.69811320754717,0.699685534591195,
0.70125786163522,0.702830188679245,0.70440251572327,0.705974842767296,0.707547169811321,
0.709119496855346,0.710691823899371,0.712264150943396,0.713836477987421,
0.715408805031447,0.716981132075472,0.718553459119497,0.720125786163522,
0.721698113207547,0.723270440251572,0.724842767295597,0.726415094339623,
0.727987421383648,0.729559748427673,0.731132075471698,0.732704402515723,
0.734276729559748,0.735849056603774,0.737421383647799,0.738993710691824,
0.740566037735849,0.742138364779874,0.743710691823899,0.745283018867924,
0.74685534591195,0.748427672955975,0.75,0.751572327044025,0.75314465408805,
0.754716981132076,0.756289308176101,0.757861635220126,0.759433962264151,
0.761006289308176,0.762578616352201,0.764150943396226,0.765723270440252,
0.767295597484277,0.768867924528302,0.770440251572327,0.772012578616352,
0.773584905660377,0.775157232704403,0.776729559748428,0.778301886792453,
0.779874213836478,0.781446540880503,0.783018867924528,0.784591194968553,
0.786163522012579,0.787735849056604,0.789308176100629,0.790880503144654,
0.792452830188679,0.794025157232704,0.79559748427673,0.797169811320755,
0.79874213836478,0.800314465408805,0.80188679245283,0.803459119496855,0.805031446540881,
0.806603773584906,0.808176100628931,0.809748427672956,0.811320754716981,
0.812893081761006,0.814465408805031,0.816037735849057,0.817610062893082,
0.819182389937107,0.820754716981132,0.822327044025157,0.823899371069182,
0.825471698113208,0.827044025157233,0.828616352201258,0.830188679245283,
0.831761006289308,0.833333333333333,0.834905660377358,0.836477987421384,
0.838050314465409,0.839622641509434,0.841194968553459,0.842767295597484,
0.844339622641509,0.845911949685535,0.84748427672956,0.849056603773585,
0.85062893081761,0.852201257861635,0.85377358490566,0.855345911949686,0.856918238993711,
0.858490566037736,0.860062893081761,0.861635220125786,0.863207547169811,
0.864779874213837,0.866352201257862,0.867924528301887,0.869496855345912,
0.871069182389937,0.872641509433962,0.874213836477987,0.875786163522013,
0.877358490566038,0.878930817610063,0.880503144654088,0.882075471698113,
0.883647798742138,0.885220125786163,0.886792452830189,0.888364779874214,
0.889937106918239,0.891509433962264,0.893081761006289,0.894654088050314,
0.89622641509434,0.897798742138365,0.89937106918239,0.900943396226415,0.90251572327044,
0.904088050314465,0.905660377358491,0.907232704402516,0.908805031446541,
0.910377358490566,0.911949685534591,0.913522012578616,0.915094339622642,
0.916666666666667,0.918238993710692,0.919811320754717,0.921383647798742,
0.922955974842767,0.924528301886792,0.926100628930818,0.927672955974843,
0.929245283018868,0.930817610062893,0.932389937106918,0.933962264150943,
0.935534591194969,0.937106918238994,0.938679245283019,0.940251572327044,
0.941823899371069,0.943396226415094,0.944968553459119,0.946540880503145,
0.94811320754717,0.949685534591195,0.95125786163522,0.952830188679245,0.95440251572327,
0.955974842767296,0.957547169811321,0.959119496855346,0.960691823899371,
0.962264150943396,0.963836477987421,0.965408805031447,0.966981132075472,
0.968553459119497,0.970125786163522,0.971698113207547,0.973270440251572,
0.974842767295597,0.976415094339623,0.977987421383648,0.979559748427673,
0.981132075471698,0.982704402515723,0.984276729559748,0.985849056603774,
0.987421383647799,0.988993710691824,0.990566037735849,0.992138364779874,
0.993710691823899,0.995283018867924,0.99685534591195,0.997310967235791),
 .UNSPECIFIED.)
GEOMETRIC_REPRESENTATION_ITEM()
RATIONAL_B_SPLINE_SURFACE(((1.,0.866025403784439,1.,0.866025403784439,1.,
0.866025403784439,1.,0.866025403784439,1.,0.866025403784439,1.,0.866025403784439,
1.,0.866025403784439,1.,0.866025403784439,1.,0.866025403784439,1.,0.866025403784439,
1.,0.866025403784439,1.,0.866025403784439,1.,0.866025403784439,1.,0.866025403784439,
1.,0.866025403784439,1.,0.866025403784439,1.,0.866025403784439,1.,0.866025403784439,
1.,0.866025403784439,1.,0.866025403784439,1.,0.866025403784439,1.,0.866025403784439,
1.,0.866025403784439,1.,0.866025403784439,1.,0.866025403784439,1.,0.866025403784439,
1.,0.866025403784439,1.,0.866025403784439,1.,0.866025403784439,1.,0.866025403784439,
1.,0.866025403784439,1.,0.866025403784439,1.,0.866025403784439,1.,0.866025403784439,
1.,0.866025403784439,1.,0.866025403784439,1.,0.866025403784439,1.,0.866025403784439,
1.,0.866025403784439,1.,0.866025403784439,1.,0.866025403784439,1.,0.866025403784439,
1.,0.866025403784439,1.,0.866025403784439,1.,0.866025403784439,1.,0.866025403784439,
1.,0.866025403784439,1.,0.866025403784439,1.,0.866025403784439,1.,0.866025403784439,
1.,0.866025403784439,1.,0.866025403784439,1.,0.866025403784439,1.,0.866025403784439,
1.,0.866025403784439,1.,0.866025403784439,1.,0.866025403784439,1.,0.866025403784439,
1.,0.866025403784439,1.,0.866025403784439,1.,0.866025403784439,1.,0.866025403784439,
1.,0.866025403784439,1.,0.866025403784439,1.,0.866025403784439,1.,0.866025403784439,
1.,0.866025403784439,1.,0.866025403784439,1.,0.866025403784439,1.,0.866025403784439,
1.,0.866025403784439,1.,0.866025403784439,1.,0.866025403784439,1.,0.866025403784439,
1.,0.866025403784439,1.,0.866025403784439,1.,0.866025403784439,1.,0.866025403784439,
1.,0.866025403784439,1.,0.866025403784439,1.,0.866025403784439,1.,0.866025403784439,
1.,0.866025403784439,1.,0.866025403784439,1.,0.866025403784439,1.,0.866025403784439,
1.,0.866025403784439,1.,0.866025403784439,1.,0.866025403784439,1.,0.866025403784439,
1.,0.866025403784439,1.,0.866025403784439,1.,0.866025403784439,1.,0.866025403784439,
1.,0.866025403784439,1.,0.866025403784439,1.,0.866025403784439,1.,0.866025403784439,
1.,0.866025403784439,1.,0.866025403784439,1.,0.866025403784439,1.,0.866025403784439,
1.,0.866025403784439,1.,0.866025403784439,1.,0.866025403784439,1.,0.866025403784439,
1.,0.866025403784439,1.,0.866025403784439,1.,0.866025403784439,1.,0.866025403784439,
1.,0.866025403784439,1.,0.866025403784439,1.,0.866025403784439,1.,0.866025403784439,
1.,0.866025403784439,1.,0.866025403784439,1.,0.866025403784439,1.,0.866025403784439,
1.,0.866025403784439,1.,0.866025403784439,1.,0.866025403784439,1.,0.866025403784439,
1.,0.866025403784439,1.,0.866025403784439,1.,0.866025403784439,1.,0.866025403784439,
1.,0.866025403784439,1.,0.866025403784439,1.,0.866025403784439,1.,0.866025403784439,
1.,0.866025403784439,1.,0.866025403784439,1.,0.866025403784439,1.,0.866025403784439,
1.,0.866025403784439,1.,0.866025403784439,1.,0.866025403784439,1.,0.866025403784439,
1.,0.866025403784439,1.,0.866025403784439,1.,0.866025403784439,1.,0.866025403784439,
1.,0.866025403784439,1.,0.866025403784439,1.,0.866025403784439,1.,0.866025403784439,
1.,0.866025403784439,1.,0.866025403784439,1.,0.866025403784439,1.,0.866025403784439,
1.,0.866025403784439,1.,0.866025403784439,1.,0.866025403784439,1.,0.866025403784439,
1.,0.866025403784439,1.,0.866025403784439,1.,0.866025403784439,1.,0.866025403784439,
1.,0.866025403784439,1.,0.866025403784439,1.,0.866025403784439,1.,0.866025403784439,
1.,0.866025403784439,1.,0.866025403784439,1.,0.866025403784439,1.,0.866025403784439,
1.,0.866025403784439,1.,0.866025403784439,1.,0.866025403784439,1.,0.866025403784439,
1.,0.866025403784439,1.,0.866025403784439,1.,0.866025403784439,1.,0.866025403784439,
1.,0.866025403784439,1.,0.866025403784439,1.,0.866025403784439,1.,0.866025403784439,
1.,0.866025403784439,1.,0.866025403784439,1.,0.866025403784439,1.,0.866025403784439,
1.,0.866025403784439,1.,0.866025403784439,1.,0.866025403784439,1.,0.866025403784439,
1.,0.866025403784439,1.,0.866025403784439,1.,0.866025403784439,1.,0.866025403784439,
1.,0.866025403784439,1.,0.866025403784439,1.,0.866025403784439,1.,0.866025403784439,
1.,0.866025403784439,1.,0.866025403784439,1.,0.866025403784439,1.,0.866025403784439,
1.,0.866025403784439,1.,0.866025403784439,1.,0.866025403784439,1.,0.866025403784439,
1.,0.866025403784439,1.,0.866025403784439,1.,0.866025403784439,1.,0.866025403784439,
1.,0.866025403784439,1.,0.866025403784439,1.,0.866025403784439,1.,0.866025403784439,
1.,0.866025403784439,1.,0.866025403784439,1.,0.866025403784439,1.,0.866025403784439,
1.,0.866025403784439,1.,0.866025403784439,1.,0.866025403784439,1.,0.866025403784439,
1.,0.866025403784439,1.,0.866025403784439,1.,0.866025403784439,1.,0.866025403784439,
1.,0.866025403784439,1.,0.866025403784439,1.,0.866025403784439,1.,0.866025403784439,
1.,0.866025403784439,1.,0.866025403784439,1.,0.866025403784439,1.,0.866025403784439,
1.,0.866025403784439,1.,0.866025403784439,1.,0.866025403784439,1.,0.866025403784439,
1.,0.866025403784439,1.,0.866025403784439,1.,0.866025403784439,1.,0.866025403784439,
1.,0.866025403784439,1.,0.866025403784439,1.,0.866025403784439,1.,0.866025403784439,
1.,0.866025403784439,1.,0.866025403784439,1.,0.866025403784439,1.,0.866025403784439,
1.,0.866025403784439,1.,0.866025403784439,1.,0.866025403784439,1.,0.866025403784439,
1.,0.866025403784439,1.,0.866025403784439,1.,0.866025403784439,1.,0.866025403784439,
1.,0.866025403784439,1.,0.866025403784439,1.,0.866025403784439,1.,0.866025403784439,
1.,0.866025403784439,1.,0.866025403784439,1.,0.866025403784439,1.,0.866025403784439,
1.,0.866025403784439,1.,0.866025403784439,1.,0.866025403784439,1.,0.866025403784439,
1.,0.866025403784439,1.,0.866025403784439,1.,0.866025403784439,1.,0.866025403784439,
1.,0.866025403784439,1.,0.866025403784439,1.,0.866025403784439,1.,0.866025403784439,
1.,0.866025403784439,1.,0.866025403784439,1.,0.866025403784439,1.,0.866025403784439,
1.,0.866025403784439,1.,0.866025403784439,1.,0.866025403784439,1.,0.866025403784439,
1.,0.866025403784439,1.,0.866025403784439,1.,0.866025403784439,1.,0.866025403784439,
1.,0.866025403784439,1.,0.866025403784439,1.,0.866025403784439,1.,0.866025403784439,
1.,0.866025403784439,1.,0.866025403784439,1.,0.866025403784439,1.,0.866025403784439,
1.,0.866025403784439,1.,0.866025403784439,1.,0.866025403784439,1.,0.866025403784439,
1.,0.866025403784439,1.,0.866025403784439,1.,0.866025403784439,1.,0.866025403784439,
1.,0.866025403784439,1.,0.866025403784439,1.,0.866025403784439,1.,0.866025403784439,
1.,0.866025403784439,1.,0.866025403784439,1.,0.866025403784439,1.,0.866025403784439,
1.,0.866025403784439,1.,0.866025403784439,1.,0.866025403784439,1.,0.866025403784439,
1.,0.866025403784439,1.,0.866025403784439,1.,0.866025403784439,1.,0.866025403784439,
1.,0.866025403784439,1.,0.866025403784439,1.,0.866025403784439,1.,0.866025403784439,
1.,0.866025403784439,1.,0.866025403784439,1.,0.866025403784439,1.,0.866025403784439,
1.,0.866025403784439,1.,0.866025403784439,1.,0.866025403784439,1.,0.866025403784439,
1.,0.866025403784439,1.,0.866025403784439,1.,0.866025403784439,1.,0.866025403784439,
1.,0.866025403784439,1.,0.866025403784439,1.,0.866025403784439,1.,0.866025403784439,
1.,0.866025403784439,1.,0.866025403784439,1.,0.866025403784439,1.,0.866025403784439,
1.,0.866025403784439,1.,0.866025403784439,1.,0.866025403784439,1.,0.866025403784439,
1.,0.866025403784439,1.,0.866025403784439,1.,0.866025403784439,1.,0.866025403784439,
1.,0.866025403784439,1.,0.866025403784439,1.,0.866025403784439,1.,0.866025403784439,
1.,0.866025403784439,1.,0.866025403784439,1.,0.866025403784439,1.,0.866025403784439,
1.,0.866025403784439,1.,0.866025403784439,1.,0.866025403784439,1.,0.866025403784439,
1.,0.866025403784439,1.,0.866025403784439,1.,0.866025403784439,1.,0.866025403784439,
1.,0.866025403784439,1.,0.866025403784439,1.,0.866025403784439,1.,0.866025403784439,
1.,0.866025403784439,1.,0.866025403784439,1.,0.866025403784439,1.,0.866025403784439,
1.,0.866025403784439,1.,0.866025403784439,1.,0.866025403784439,1.,0.866025403784439,
1.,0.866025403784439,1.,0.866025403784439,1.,0.866025403784439,1.,0.866025403784439,
1.,0.866025403784439,1.,0.866025403784439,1.,0.866025403784439,1.,0.866025403784439,
1.,0.866025403784439,1.,0.866025403784439,1.,0.866025403784439,1.,0.866025403784439,
1.,0.866025403784439,1.,0.866025403784439,1.,0.866025403784439,1.,0.866025403784439,
1.,0.866025403784439,1.,0.866025403784439,1.,0.866025403784439,1.,0.866025403784439,
1.,0.866025403784439,1.,0.866025403784439,1.,0.866025403784439,1.,0.866025403784439,
1.,0.866025403784439,1.,0.866025403784439,1.,0.866025403784439,1.,0.866025403784439,
1.,0.866025403784439,1.,0.866025403784439,1.,0.866025403784439,1.,0.866025403784439,
1.,0.866025403784439,1.,0.866025403784439,1.,0.866025403784439,1.,0.866025403784439,
1.,0.866025403784439,1.,0.866025403784439,1.,0.866025403784439,1.,0.866025403784439,
1.,0.866025403784439,1.,0.866025403784439,1.,0.866025403784439,1.,0.866025403784439,
1.,0.866025403784439,1.,0.866025403784439,1.,0.866025403784439,1.,0.866025403784439,
1.,0.866025403784439,1.,0.866025403784439,1.,0.866025403784439,1.,0.866025403784439,
1.,0.866025403784439,1.,0.866025403784439,1.,0.866025403784439,1.,0.866025403784439,
1.,0.866025403784439,1.,0.866025403784439,1.,0.866025403784439,1.,0.866025403784439,
1.,0.866025403784439,1.,0.866025403784439,1.,0.866025403784439,1.,0.866025403784439,
1.,0.866025403784439,1.,0.866025403784439,1.,0.866025403784439,1.,0.866025403784439,
1.,0.866025403784439,1.,0.866025403784439,1.,0.866025403784439,1.,0.866025403784439,
1.,0.866025403784439,1.,0.866025403784439,1.,0.866025403784439,1.,0.866025403784439,
1.,0.866025403784439,1.,0.866025403784439,1.,0.866025403784439,1.,0.866025403784439,
1.,0.866025403784439,1.,0.866025403784439,1.,0.866025403784439,1.,0.866025403784439,
1.,0.866025403784439,1.,0.866025403784439,1.,0.866025403784439,1.,0.866025403784439,
1.,0.866025403784439,1.,0.866025403784439,1.,0.866025403784439,1.,0.866025403784439,
1.,0.866025403784439,1.,0.866025403784439,1.,0.866025403784439,1.,0.866025403784439,
1.,0.866025403784439,1.,0.866025403784439,1.,0.866025403784439,1.,0.866025403784439,
1.,0.866025403784439,1.,0.866025403784439,1.,0.866025403784439,1.,0.866025403784439,
1.,0.866025403784439,1.,0.866025403784439,1.,0.866025403784439,1.,0.866025403784439,
1.,0.866025403784439,1.,0.866025403784439,1.,0.866025403784439,1.,0.866025403784439,
1.,0.866025403784439,1.,0.866025403784439,1.,0.866025403784439,1.,0.866025403784439,
1.,0.866025403784439,1.,0.866025403784439,1.,0.866025403784439,1.,0.866025403784439,
1.,0.866025403784439,1.,0.866025403784439,1.,0.866025403784439,1.,0.866025403784439,
1.,0.866025403784439,1.,0.866025403784439,1.,0.866025403784439,1.,0.866025403784439,
1.,0.866025403784439,1.,0.866025403784439,1.,0.866025403784439,1.,0.866025403784439,
1.,0.866025403784439,1.,0.866025403784439,1.,0.866025403784439,1.,0.866025403784439,
1.,0.866025403784439,1.,0.866025403784439,1.,0.866025403784439,1.,0.866025403784439,
1.,0.866025403784439,1.,0.866025403784439,1.,0.866025403784439,1.,0.866025403784439,
1.,0.866025403784439,1.,0.866025403784439,1.,0.866025403784439,1.,0.866025403784439,
1.,0.866025403784439,1.,0.866025403784439,1.,0.866025403784439,1.,0.866025403784439,
1.,0.866025403784439,1.,0.866025403784439,1.,0.866025403784439,1.,0.866025403784439,
1.,0.866025403784439,1.,0.866025403784439,1.,0.866025403784439,1.,0.866025403784439,
1.,0.866025403784439,1.,0.866025403784439,1.,0.866025403784439,1.,0.866025403784439,
1.,0.866025403784439,1.,0.866025403784439,1.,0.866025403784439,1.,0.866025403784439,
1.,0.866025403784439,1.,0.866025403784439,1.,0.866025403784439,1.,0.866025403784439,
1.,0.866025403784439,1.,0.866025403784439,1.,0.866025403784439,1.,0.866025403784439,
1.,0.866025403784439,1.,0.866025403784439,1.,0.866025403784439,1.,0.866025403784439,
1.,0.866025403784439,1.,0.866025403784439,1.,0.866025403784439,1.,0.866025403784439,
1.,0.866025403784439,1.,0.866025403784439,1.,0.866025403784439,1.,0.866025403784439,
1.,0.866025403784439,1.,0.866025403784439,1.,0.866025403784439,1.,0.866025403784439,
1.,0.866025403784439,1.,0.866025403784439,1.,0.866025403784439,1.,0.866025403784439,
1.,0.866025403784439,1.,0.866025403784439,1.,0.866025403784439,1.,0.866025403784439,
1.,0.866025403784439,1.,0.866025403784439,1.,0.866025403784439,1.,0.866025403784439,
1.,0.866025403784439,1.,0.866025403784439,1.,0.866025403784439,1.,0.866025403784439,
1.,0.866025403784439,1.,0.866025403784439,1.,0.866025403784439,1.,0.866025403784439,
1.,0.866025403784439,1.,0.866025403784439,1.,0.866025403784439,1.,0.866025403784439,
1.,0.866025403784439,1.,0.866025403784439,1.,0.866025403784439,1.,0.866025403784439,
1.,0.866025403784439,1.,0.866025403784439,1.,0.866025403784439,1.,0.866025403784439,
1.,0.866025403784439,1.,0.866025403784439,1.,0.866025403784439,1.,0.866025403784439,
1.,0.866025403784439,1.,0.866025403784439,1.,0.866025403784439,1.,0.866025403784439,
1.,0.866025403784439,1.,0.866025403784439,1.,0.866025403784439,1.,0.866025403784439,
1.,0.866025403784439,1.,0.866025403784439,1.,0.866025403784439,1.,0.866025403784439,
1.,0.866025403784439,1.,0.866025403784439,1.,0.866025403784439,1.,0.866025403784439,
1.,0.866025403784439,1.,0.866025403784439,1.,0.866025403784439,1.,0.866025403784439,
1.,0.866025403784439,1.,0.866025403784439,1.,0.866025403784439,1.,0.866025403784439,
1.,0.866025403784439,1.,0.866025403784439,1.,0.866025403784439,1.,0.866025403784439,
1.,0.961177489682721,0.944854577795434),(1.,0.866025403784439,1.,0.866025403784439,
1.,0.866025403784439,1.,0.866025403784439,1.,0.866025403784439,1.,0.866025403784439,
1.,0.866025403784439,1.,0.866025403784439,1.,0.866025403784439,1.,0.866025403784439,
1.,0.866025403784439,1.,0.866025403784439,1.,0.866025403784439,1.,0.866025403784439,
1.,0.866025403784439,1.,0.866025403784439,1.,0.866025403784439,1.,0.866025403784439,
1.,0.866025403784439,1.,0.866025403784439,1.,0.866025403784439,1.,0.866025403784439,
1.,0.866025403784439,1.,0.866025403784439,1.,0.866025403784439,1.,0.866025403784439,
1.,0.866025403784439,1.,0.866025403784439,1.,0.866025403784439,1.,0.866025403784439,
1.,0.866025403784439,1.,0.866025403784439,1.,0.866025403784439,1.,0.866025403784439,
1.,0.866025403784439,1.,0.866025403784439,1.,0.866025403784439,1.,0.866025403784439,
1.,0.866025403784439,1.,0.866025403784439,1.,0.866025403784439,1.,0.866025403784439,
1.,0.866025403784439,1.,0.866025403784439,1.,0.866025403784439,1.,0.866025403784439,
1.,0.866025403784439,1.,0.866025403784439,1.,0.866025403784439,1.,0.866025403784439,
1.,0.866025403784439,1.,0.866025403784439,1.,0.866025403784439,1.,0.866025403784439,
1.,0.866025403784439,1.,0.866025403784439,1.,0.866025403784439,1.,0.866025403784439,
1.,0.866025403784439,1.,0.866025403784439,1.,0.866025403784439,1.,0.866025403784439,
1.,0.866025403784439,1.,0.866025403784439,1.,0.866025403784439,1.,0.866025403784439,
1.,0.866025403784439,1.,0.866025403784439,1.,0.866025403784439,1.,0.866025403784439,
1.,0.866025403784439,1.,0.866025403784439,1.,0.866025403784439,1.,0.866025403784439,
1.,0.866025403784439,1.,0.866025403784439,1.,0.866025403784439,1.,0.866025403784439,
1.,0.866025403784439,1.,0.866025403784439,1.,0.866025403784439,1.,0.866025403784439,
1.,0.866025403784439,1.,0.866025403784439,1.,0.866025403784439,1.,0.866025403784439,
1.,0.866025403784439,1.,0.866025403784439,1.,0.866025403784439,1.,0.866025403784439,
1.,0.866025403784439,1.,0.866025403784439,1.,0.866025403784439,1.,0.866025403784439,
1.,0.866025403784439,1.,0.866025403784439,1.,0.866025403784439,1.,0.866025403784439,
1.,0.866025403784439,1.,0.866025403784439,1.,0.866025403784439,1.,0.866025403784439,
1.,0.866025403784439,1.,0.866025403784439,1.,0.866025403784439,1.,0.866025403784439,
1.,0.866025403784439,1.,0.866025403784439,1.,0.866025403784439,1.,0.866025403784439,
1.,0.866025403784439,1.,0.866025403784439,1.,0.866025403784439,1.,0.866025403784439,
1.,0.866025403784439,1.,0.866025403784439,1.,0.866025403784439,1.,0.866025403784439,
1.,0.866025403784439,1.,0.866025403784439,1.,0.866025403784439,1.,0.866025403784439,
1.,0.866025403784439,1.,0.866025403784439,1.,0.866025403784439,1.,0.866025403784439,
1.,0.866025403784439,1.,0.866025403784439,1.,0.866025403784439,1.,0.866025403784439,
1.,0.866025403784439,1.,0.866025403784439,1.,0.866025403784439,1.,0.866025403784439,
1.,0.866025403784439,1.,0.866025403784439,1.,0.866025403784439,1.,0.866025403784439,
1.,0.866025403784439,1.,0.866025403784439,1.,0.866025403784439,1.,0.866025403784439,
1.,0.866025403784439,1.,0.866025403784439,1.,0.866025403784439,1.,0.866025403784439,
1.,0.866025403784439,1.,0.866025403784439,1.,0.866025403784439,1.,0.866025403784439,
1.,0.866025403784439,1.,0.866025403784439,1.,0.866025403784439,1.,0.866025403784439,
1.,0.866025403784439,1.,0.866025403784439,1.,0.866025403784439,1.,0.866025403784439,
1.,0.866025403784439,1.,0.866025403784439,1.,0.866025403784439,1.,0.866025403784439,
1.,0.866025403784439,1.,0.866025403784439,1.,0.866025403784439,1.,0.866025403784439,
1.,0.866025403784439,1.,0.866025403784439,1.,0.866025403784439,1.,0.866025403784439,
1.,0.866025403784439,1.,0.866025403784439,1.,0.866025403784439,1.,0.866025403784439,
1.,0.866025403784439,1.,0.866025403784439,1.,0.866025403784439,1.,0.866025403784439,
1.,0.866025403784439,1.,0.866025403784439,1.,0.866025403784439,1.,0.866025403784439,
1.,0.866025403784439,1.,0.866025403784439,1.,0.866025403784439,1.,0.866025403784439,
1.,0.866025403784439,1.,0.866025403784439,1.,0.866025403784439,1.,0.866025403784439,
1.,0.866025403784439,1.,0.866025403784439,1.,0.866025403784439,1.,0.866025403784439,
1.,0.866025403784439,1.,0.866025403784439,1.,0.866025403784439,1.,0.866025403784439,
1.,0.866025403784439,1.,0.866025403784439,1.,0.866025403784439,1.,0.866025403784439,
1.,0.866025403784439,1.,0.866025403784439,1.,0.866025403784439,1.,0.866025403784439,
1.,0.866025403784439,1.,0.866025403784439,1.,0.866025403784439,1.,0.866025403784439,
1.,0.866025403784439,1.,0.866025403784439,1.,0.866025403784439,1.,0.866025403784439,
1.,0.866025403784439,1.,0.866025403784439,1.,0.866025403784439,1.,0.866025403784439,
1.,0.866025403784439,1.,0.866025403784439,1.,0.866025403784439,1.,0.866025403784439,
1.,0.866025403784439,1.,0.866025403784439,1.,0.866025403784439,1.,0.866025403784439,
1.,0.866025403784439,1.,0.866025403784439,1.,0.866025403784439,1.,0.866025403784439,
1.,0.866025403784439,1.,0.866025403784439,1.,0.866025403784439,1.,0.866025403784439,
1.,0.866025403784439,1.,0.866025403784439,1.,0.866025403784439,1.,0.866025403784439,
1.,0.866025403784439,1.,0.866025403784439,1.,0.866025403784439,1.,0.866025403784439,
1.,0.866025403784439,1.,0.866025403784439,1.,0.866025403784439,1.,0.866025403784439,
1.,0.866025403784439,1.,0.866025403784439,1.,0.866025403784439,1.,0.866025403784439,
1.,0.866025403784439,1.,0.866025403784439,1.,0.866025403784439,1.,0.866025403784439,
1.,0.866025403784439,1.,0.866025403784439,1.,0.866025403784439,1.,0.866025403784439,
1.,0.866025403784439,1.,0.866025403784439,1.,0.866025403784439,1.,0.866025403784439,
1.,0.866025403784439,1.,0.866025403784439,1.,0.866025403784439,1.,0.866025403784439,
1.,0.866025403784439,1.,0.866025403784439,1.,0.866025403784439,1.,0.866025403784439,
1.,0.866025403784439,1.,0.866025403784439,1.,0.866025403784439,1.,0.866025403784439,
1.,0.866025403784439,1.,0.866025403784439,1.,0.866025403784439,1.,0.866025403784439,
1.,0.866025403784439,1.,0.866025403784439,1.,0.866025403784439,1.,0.866025403784439,
1.,0.866025403784439,1.,0.866025403784439,1.,0.866025403784439,1.,0.866025403784439,
1.,0.866025403784439,1.,0.866025403784439,1.,0.866025403784439,1.,0.866025403784439,
1.,0.866025403784439,1.,0.866025403784439,1.,0.866025403784439,1.,0.866025403784439,
1.,0.866025403784439,1.,0.866025403784439,1.,0.866025403784439,1.,0.866025403784439,
1.,0.866025403784439,1.,0.866025403784439,1.,0.866025403784439,1.,0.866025403784439,
1.,0.866025403784439,1.,0.866025403784439,1.,0.866025403784439,1.,0.866025403784439,
1.,0.866025403784439,1.,0.866025403784439,1.,0.866025403784439,1.,0.866025403784439,
1.,0.866025403784439,1.,0.866025403784439,1.,0.866025403784439,1.,0.866025403784439,
1.,0.866025403784439,1.,0.866025403784439,1.,0.866025403784439,1.,0.866025403784439,
1.,0.866025403784439,1.,0.866025403784439,1.,0.866025403784439,1.,0.866025403784439,
1.,0.866025403784439,1.,0.866025403784439,1.,0.866025403784439,1.,0.866025403784439,
1.,0.866025403784439,1.,0.866025403784439,1.,0.866025403784439,1.,0.866025403784439,
1.,0.866025403784439,1.,0.866025403784439,1.,0.866025403784439,1.,0.866025403784439,
1.,0.866025403784439,1.,0.866025403784439,1.,0.866025403784439,1.,0.866025403784439,
1.,0.866025403784439,1.,0.866025403784439,1.,0.866025403784439,1.,0.866025403784439,
1.,0.866025403784439,1.,0.866025403784439,1.,0.866025403784439,1.,0.866025403784439,
1.,0.866025403784439,1.,0.866025403784439,1.,0.866025403784439,1.,0.866025403784439,
1.,0.866025403784439,1.,0.866025403784439,1.,0.866025403784439,1.,0.866025403784439,
1.,0.866025403784439,1.,0.866025403784439,1.,0.866025403784439,1.,0.866025403784439,
1.,0.866025403784439,1.,0.866025403784439,1.,0.866025403784439,1.,0.866025403784439,
1.,0.866025403784439,1.,0.866025403784439,1.,0.866025403784439,1.,0.866025403784439,
1.,0.866025403784439,1.,0.866025403784439,1.,0.866025403784439,1.,0.866025403784439,
1.,0.866025403784439,1.,0.866025403784439,1.,0.866025403784439,1.,0.866025403784439,
1.,0.866025403784439,1.,0.866025403784439,1.,0.866025403784439,1.,0.866025403784439,
1.,0.866025403784439,1.,0.866025403784439,1.,0.866025403784439,1.,0.866025403784439,
1.,0.866025403784439,1.,0.866025403784439,1.,0.866025403784439,1.,0.866025403784439,
1.,0.866025403784439,1.,0.866025403784439,1.,0.866025403784439,1.,0.866025403784439,
1.,0.866025403784439,1.,0.866025403784439,1.,0.866025403784439,1.,0.866025403784439,
1.,0.866025403784439,1.,0.866025403784439,1.,0.866025403784439,1.,0.866025403784439,
1.,0.866025403784439,1.,0.866025403784439,1.,0.866025403784439,1.,0.866025403784439,
1.,0.866025403784439,1.,0.866025403784439,1.,0.866025403784439,1.,0.866025403784439,
1.,0.866025403784439,1.,0.866025403784439,1.,0.866025403784439,1.,0.866025403784439,
1.,0.866025403784439,1.,0.866025403784439,1.,0.866025403784439,1.,0.866025403784439,
1.,0.866025403784439,1.,0.866025403784439,1.,0.866025403784439,1.,0.866025403784439,
1.,0.866025403784439,1.,0.866025403784439,1.,0.866025403784439,1.,0.866025403784439,
1.,0.866025403784439,1.,0.866025403784439,1.,0.866025403784439,1.,0.866025403784439,
1.,0.866025403784439,1.,0.866025403784439,1.,0.866025403784439,1.,0.866025403784439,
1.,0.866025403784439,1.,0.866025403784439,1.,0.866025403784439,1.,0.866025403784439,
1.,0.866025403784439,1.,0.866025403784439,1.,0.866025403784439,1.,0.866025403784439,
1.,0.866025403784439,1.,0.866025403784439,1.,0.866025403784439,1.,0.866025403784439,
1.,0.866025403784439,1.,0.866025403784439,1.,0.866025403784439,1.,0.866025403784439,
1.,0.866025403784439,1.,0.866025403784439,1.,0.866025403784439,1.,0.866025403784439,
1.,0.866025403784439,1.,0.866025403784439,1.,0.866025403784439,1.,0.866025403784439,
1.,0.866025403784439,1.,0.866025403784439,1.,0.866025403784439,1.,0.866025403784439,
1.,0.866025403784439,1.,0.866025403784439,1.,0.866025403784439,1.,0.866025403784439,
1.,0.866025403784439,1.,0.866025403784439,1.,0.866025403784439,1.,0.866025403784439,
1.,0.866025403784439,1.,0.866025403784439,1.,0.866025403784439,1.,0.866025403784439,
1.,0.866025403784439,1.,0.866025403784439,1.,0.866025403784439,1.,0.866025403784439,
1.,0.866025403784439,1.,0.866025403784439,1.,0.866025403784439,1.,0.866025403784439,
1.,0.866025403784439,1.,0.866025403784439,1.,0.866025403784439,1.,0.866025403784439,
1.,0.866025403784439,1.,0.866025403784439,1.,0.866025403784439,1.,0.866025403784439,
1.,0.866025403784439,1.,0.866025403784439,1.,0.866025403784439,1.,0.866025403784439,
1.,0.866025403784439,1.,0.866025403784439,1.,0.866025403784439,1.,0.866025403784439,
1.,0.866025403784439,1.,0.866025403784439,1.,0.866025403784439,1.,0.866025403784439,
1.,0.866025403784439,1.,0.866025403784439,1.,0.866025403784439,1.,0.866025403784439,
1.,0.866025403784439,1.,0.866025403784439,1.,0.866025403784439,1.,0.866025403784439,
1.,0.866025403784439,1.,0.866025403784439,1.,0.866025403784439,1.,0.866025403784439,
1.,0.866025403784439,1.,0.866025403784439,1.,0.866025403784439,1.,0.866025403784439,
1.,0.866025403784439,1.,0.866025403784439,1.,0.866025403784439,1.,0.866025403784439,
1.,0.866025403784439,1.,0.866025403784439,1.,0.866025403784439,1.,0.866025403784439,
1.,0.866025403784439,1.,0.866025403784439,1.,0.866025403784439,1.,0.866025403784439,
1.,0.866025403784439,1.,0.866025403784439,1.,0.866025403784439,1.,0.866025403784439,
1.,0.866025403784439,1.,0.866025403784439,1.,0.866025403784439,1.,0.866025403784439,
1.,0.866025403784439,1.,0.866025403784439,1.,0.866025403784439,1.,0.866025403784439,
1.,0.866025403784439,1.,0.866025403784439,1.,0.866025403784439,1.,0.866025403784439,
1.,0.866025403784439,1.,0.866025403784439,1.,0.866025403784439,1.,0.866025403784439,
1.,0.866025403784439,1.,0.866025403784439,1.,0.866025403784439,1.,0.866025403784439,
1.,0.866025403784439,1.,0.866025403784439,1.,0.866025403784439,1.,0.866025403784439,
1.,0.866025403784439,1.,0.866025403784439,1.,0.866025403784439,1.,0.866025403784439,
1.,0.866025403784439,1.,0.866025403784439,1.,0.866025403784439,1.,0.866025403784439,
1.,0.866025403784439,1.,0.866025403784439,1.,0.866025403784439,1.,0.866025403784439,
1.,0.866025403784439,1.,0.866025403784439,1.,0.866025403784439,1.,0.866025403784439,
1.,0.866025403784439,1.,0.866025403784439,1.,0.866025403784439,1.,0.866025403784439,
1.,0.866025403784439,1.,0.866025403784439,1.,0.866025403784439,1.,0.866025403784439,
1.,0.866025403784439,1.,0.866025403784439,1.,0.866025403784439,1.,0.866025403784439,
1.,0.866025403784439,1.,0.866025403784439,1.,0.866025403784439,1.,0.866025403784439,
1.,0.866025403784439,1.,0.866025403784439,1.,0.866025403784439,1.,0.866025403784439,
1.,0.866025403784439,1.,0.866025403784439,1.,0.866025403784439,1.,0.866025403784439,
1.,0.866025403784439,1.,0.866025403784439,1.,0.866025403784439,1.,0.866025403784439,
1.,0.866025403784439,1.,0.866025403784439,1.,0.866025403784439,1.,0.866025403784439,
1.,0.866025403784439,1.,0.866025403784439,1.,0.866025403784439,1.,0.866025403784439,
1.,0.866025403784439,1.,0.866025403784439,1.,0.866025403784439,1.,0.866025403784439,
1.,0.866025403784439,1.,0.866025403784439,1.,0.866025403784439,1.,0.866025403784439,
1.,0.866025403784439,1.,0.866025403784439,1.,0.866025403784439,1.,0.866025403784439,
1.,0.866025403784439,1.,0.866025403784439,1.,0.866025403784439,1.,0.866025403784439,
1.,0.866025403784439,1.,0.866025403784439,1.,0.866025403784439,1.,0.866025403784439,
1.,0.866025403784439,1.,0.866025403784439,1.,0.866025403784439,1.,0.866025403784439,
1.,0.866025403784439,1.,0.866025403784439,1.,0.866025403784439,1.,0.866025403784439,
1.,0.961177489682721,0.944854577795434)))
REPRESENTATION_ITEM('')
SURFACE()
);
#65=B_SPLINE_CURVE_WITH_KNOTS('',3,(#3540,#3541,#3542,#3543,#3544,#3545,
#3546,#3547,#3548,#3549,#3550,#3551,#3552,#3553,#3554,#3555,#3556,#3557,
#3558,#3559),.UNSPECIFIED.,.F.,.F.,(4,2,2,2,2,2,2,2,2,4),(-0.622449302504414,
-0.602698010393903,-0.526004880371973,-0.445959911298277,-0.367327050519426,
-0.291259341940103,-0.211590365655144,-0.133821287178804,-0.0681146419635469,
-2.00520727152319E-5),.UNSPECIFIED.);
#66=B_SPLINE_CURVE_WITH_KNOTS('',3,(#3569,#3570,#3571,#3572,#3573,#3574,
#3575,#3576,#3577,#3578,#3579,#3580,#3581,#3582,#3583,#3584),
 .UNSPECIFIED.,.F.,.F.,(4,2,2,2,2,2,2,4),(-0.462334159991009,-0.394668919789225,
-0.328266148938867,-0.252215701312488,-0.17329149580553,-0.0971873778249495,
-0.0493231403597584,-3.47740632798757E-5),.UNSPECIFIED.);
#67=B_SPLINE_CURVE_WITH_KNOTS('',3,(#3589,#3590,#3591,#3592,#3593,#3594,
#3595,#3596,#3597,#3598,#3599,#3600,#3601,#3602,#3603,#3604,#3605,#3606,
#3607,#3608,#3609,#3610,#3611,#3612,#3613,#3614,#3615,#3616,#3617,#3618,
#3619,#3620,#3621,#3622,#3623,#3624),.UNSPECIFIED.,.F.,.F.,(4,2,2,2,2,2,
2,2,2,2,2,2,2,2,2,2,2,4),(-1.88592410587206,-1.85408617146932,-1.7777971269776,
-1.69806748653657,-1.61972768584256,-1.54333501691836,-1.46281579632766,
-1.38537641266744,-1.30740264102123,-1.22789473761476,-1.15136658423606,
-1.07167820080295,-0.993215731607202,-0.917046017721851,-0.837334341285013,
-0.759740251060977,-0.682391259072564,-0.622449302504414),.UNSPECIFIED.);
#68=B_SPLINE_CURVE_WITH_KNOTS('',3,(#3625,#3626,#3627,#3628,#3629,#3630,
#3631,#3632,#3633,#3634,#3635,#3636,#3637,#3638,#3639,#3640,#3641,#3642,
#3643,#3644,#3645,#3646,#3647,#3648,#3649,#3650,#3651,#3652,#3653,#3654,
#3655,#3656,#3657,#3658,#3659,#3660),.UNSPECIFIED.,.F.,.F.,(4,2,2,2,2,2,
2,2,2,2,2,2,2,2,2,2,2,4),(-15.8059078484382,-15.7284811974429,-15.653665517221,
-15.5754272842413,-15.4956816545495,-15.4194524679912,-15.3403583161977,
-15.2615169409565,-15.1844370832093,-15.1043175204315,-15.0275796663467,
-14.949602957522,-14.869883690514,-14.7937631863142,-14.7149253060571,-14.6353699334314,
-14.5585040517355,-14.5425064158919),.UNSPECIFIED.);
#69=B_SPLINE_CURVE_WITH_KNOTS('',3,(#3665,#3666,#3667,#3668,#3669,#3670,
#3671,#3672,#3673,#3674,#3675,#3676,#3677,#3678,#3679,#3680,#3681,#3682,
#3683,#3684,#3685,#3686,#3687,#3688,#3689,#3690,#3691,#3692,#3693,#3694,
#3695,#3696,#3697,#3698,#3699,#3700),.UNSPECIFIED.,.F.,.F.,(4,2,2,2,2,2,
2,2,2,2,2,2,2,2,2,2,2,4),(-3.14856413016895,-3.10489715100778,-3.02882540004088,
-2.94914924352566,-2.87133041628292,-2.79447109853634,-2.71452323561515,
-2.63760099185768,-2.55846074620274,-2.47954611547811,-2.40343190159831,
-2.32375077684371,-2.24569432443027,-2.16913428536013,-2.08892367482231,
-2.01176419496968,-1.93327835509454,-1.88592410587206),.UNSPECIFIED.);
#70=B_SPLINE_CURVE_WITH_KNOTS('',3,(#3701,#3702,#3703,#3704,#3705,#3706,
#3707,#3708,#3709,#3710,#3711,#3712,#3713,#3714,#3715,#3716,#3717,#3718,
#3719,#3720,#3721,#3722,#3723,#3724,#3725,#3726,#3727,#3728,#3729,#3730,
#3731,#3732,#3733,#3734,#3735,#3736),.UNSPECIFIED.,.F.,.F.,(4,2,2,2,2,2,
2,2,2,2,2,2,2,2,2,2,2,4),(-14.5425064158919,-14.4786220808176,-14.4015249062871,
-14.3237607179729,-14.2440259604515,-14.1678844570661,-14.0892544615079,
-14.0088975164845,-13.9321945193582,-13.8524947872604,-13.7749409217465,
-13.6973342483475,-13.6175448741017,-13.5412682628649,-13.4627911009055,
-13.3830294511391,-13.3064818519847,-13.2786570707264),.UNSPECIFIED.);
#71=B_SPLINE_CURVE_WITH_KNOTS('',3,(#3741,#3742,#3743,#3744,#3745,#3746,
#3747,#3748,#3749,#3750,#3751,#3752,#3753,#3754,#3755,#3756,#3757,#3758,
#3759,#3760,#3761,#3762,#3763,#3764,#3765,#3766,#3767,#3768,#3769,#3770,
#3771,#3772,#3773,#3774,#3775,#3776),.UNSPECIFIED.,.F.,.F.,(4,2,2,2,2,2,
2,2,2,2,2,2,2,2,2,2,2,4),(-4.41185428584948,-4.3572695192111,-4.28091869991991,
-4.2003622348938,-4.12289038795177,-4.04502319430417,-3.96547714842458,
-3.8889144417926,-3.80922320997531,-3.73072226209172,-3.65456967880987,
-3.57485814630795,-3.49722481002858,-3.41995305829719,-3.340215623117,-3.26348228462995,
-3.18357901441996,-3.14856413016895),.UNSPECIFIED.);
#72=B_SPLINE_CURVE_WITH_KNOTS('',3,(#3777,#3778,#3779,#3780,#3781,#3782,
#3783,#3784,#3785,#3786,#3787,#3788,#3789,#3790,#3791,#3792,#3793,#3794,
#3795,#3796,#3797,#3798,#3799,#3800,#3801,#3802,#3803,#3804,#3805,#3806,
#3807,#3808,#3809,#3810,#3811,#3812),.UNSPECIFIED.,.F.,.F.,(4,2,2,2,2,2,
2,2,2,2,2,2,2,2,2,2,2,4),(-13.2786570707264,-13.2269572259644,-13.1487311386957,
-13.0712676976676,-12.9907288947824,-12.9141887326979,-12.8358248605999,
-12.7559984258067,-12.6796649388668,-12.6004455529773,-12.5216609022194,
-12.4444654353247,-12.3642224886698,-12.287473412726,-12.2093801513485,
-12.1295887274691,-12.053390175169,-12.0137481254518),.UNSPECIFIED.);
#73=B_SPLINE_CURVE_WITH_KNOTS('',3,(#3817,#3818,#3819,#3820,#3821,#3822,
#3823,#3824,#3825,#3826,#3827,#3828,#3829,#3830,#3831,#3832,#3833,#3834,
#3835,#3836,#3837,#3838,#3839,#3840,#3841,#3842,#3843,#3844,#3845,#3846,
#3847,#3848,#3849,#3850,#3851,#3852),.UNSPECIFIED.,.F.,.F.,(4,2,2,2,2,2,
2,2,2,2,2,2,2,2,2,2,2,4),(-5.67436912094876,-5.60860430470927,-5.53183780362614,
-5.45186994916378,-5.37493132522109,-5.29595326180489,-5.21701483115353,
-5.14090272904409,-5.06124241308089,-4.98316085041372,-4.90666931989548,
-4.8264294684555,-4.74924503691536,-4.67089592646034,-4.59167221241137,
-4.51536004512522,-4.43564240150157,-4.41185428584948),.UNSPECIFIED.);
#74=B_SPLINE_CURVE_WITH_KNOTS('',3,(#3853,#3854,#3855,#3856,#3857,#3858,
#3859,#3860,#3861,#3862,#3863,#3864,#3865,#3866,#3867,#3868,#3869,#3870,
#3871,#3872,#3873,#3874,#3875,#3876,#3877,#3878,#3879,#3880,#3881,#3882,
#3883,#3884,#3885,#3886,#3887,#3888),.UNSPECIFIED.,.F.,.F.,(4,2,2,2,2,2,
2,2,2,2,2,2,2,2,2,2,2,4),(-12.0137481254518,-11.9744359470122,-11.8949588787454,
-11.8179869666914,-11.7379919855391,-11.6609061237253,-11.5830357049354,
-11.5032367518886,-11.4270418099655,-11.3483057128929,-11.2680400224234,
-11.1912415811657,-11.1114403116993,-11.0339137135885,-10.9562121549183,
-10.8763660484795,-10.800056548405,-10.7491628692134),.UNSPECIFIED.);
#75=B_SPLINE_CURVE_WITH_KNOTS('',3,(#3893,#3894,#3895,#3896,#3897,#3898,
#3899,#3900,#3901,#3902,#3903,#3904,#3905,#3906,#3907,#3908,#3909,#3910,
#3911,#3912,#3913,#3914,#3915,#3916,#3917,#3918,#3919,#3920,#3921,#3922,
#3923,#3924,#3925,#3926,#3927,#3928),.UNSPECIFIED.,.F.,.F.,(4,2,2,2,2,2,
2,2,2,2,2,2,2,2,2,2,2,4),(-6.93678766774197,-6.85961386328993,-6.7818900142282,
-6.70234030795459,-6.62577637948793,-6.5461183676422,-6.46761316913563,
-6.39151035618055,-6.31183531759777,-6.23419654946404,-6.15703732358235,
-6.07729038628634,-6.00055034959348,-5.92082722654057,-5.84213067069773,
-5.76608624718667,-5.68643900560237,-5.67436912094876),.UNSPECIFIED.);
#76=B_SPLINE_CURVE_WITH_KNOTS('',3,(#3929,#3930,#3931,#3932,#3933,#3934,
#3935,#3936,#3937,#3938,#3939,#3940,#3941,#3942,#3943,#3944,#3945,#3946,
#3947,#3948,#3949,#3950,#3951,#3952,#3953,#3954,#3955,#3956,#3957,#3958,
#3959,#3960,#3961,#3962,#3963,#3964),.UNSPECIFIED.,.F.,.F.,(4,2,2,2,2,2,
2,2,2,2,2,2,2,2,2,2,2,4),(-10.7491628692134,-10.721484683818,-10.6416636053348,
-10.5650269069308,-10.4854075391908,-10.407237710163,-10.329686918681,-10.2490538966559,
-10.1725061967339,-10.0940538094768,-10.014182649809,-9.93777708958984,
-9.85847000380012,-9.77976984720712,-9.70249493208427,-9.62216623393326,
-9.54543533647372,-9.48343899875196),.UNSPECIFIED.);
#77=B_SPLINE_CURVE_WITH_KNOTS('',3,(#3969,#3970,#3971,#3972,#3973,#3974,
#3975,#3976,#3977,#3978,#3979,#3980,#3981,#3982,#3983,#3984,#3985,#3986,
#3987,#3988,#3989,#3990,#3991,#3992,#3993,#3994,#3995,#3996,#3997,#3998,
#3999,#4000,#4001,#4002,#4003,#4004,#4005,#4006),.UNSPECIFIED.,.F.,.F.,
(4,2,2,2,2,2,2,2,2,2,2,2,2,2,2,2,2,2,4),(-8.19874268237018,-8.18783288474684,
-8.11091176744568,-8.03213823044703,-7.9532105718062,-7.87713164764008,
-7.79752959642434,-7.71945696582131,-7.64306894803688,-7.56283468402714,
-7.48565903996338,-7.40748596661602,-7.32826524264494,-7.25196001383447,
-7.17229117661081,-7.09391918147949,-7.01764348240122,-6.937084532239,-6.93678766774197),
 .UNSPECIFIED.);
#78=B_SPLINE_CURVE_WITH_KNOTS('',3,(#4007,#4008,#4009,#4010,#4011,#4012,
#4013,#4014,#4015,#4016,#4017,#4018,#4019,#4020,#4021,#4022,#4023,#4024,
#4025,#4026,#4027,#4028,#4029,#4030,#4031,#4032,#4033,#4034,#4035,#4036,
#4037,#4038,#4039,#4040,#4041,#4042),.UNSPECIFIED.,.F.,.F.,(4,2,2,2,2,2,
2,2,2,2,2,2,2,2,2,2,2,4),(-9.48343899875196,-9.4672619853537,-9.38743432009354,
-9.31118896360937,-9.23215524393813,-9.15278522986094,-9.0757428182935,
-8.9956717661025,-8.91862693582825,-8.84068607390281,-8.76085868335287,
-8.68464121549572,-8.60583518265837,-8.52569108674793,-8.44883212217652,
-8.36896559366926,-8.29149686349102,-8.21851276396746),.UNSPECIFIED.);
#79=B_SPLINE_CURVE_WITH_KNOTS('',3,(#4047,#4048,#4049,#4050,#4051,#4052,
#4053,#4054,#4055,#4056,#4057,#4058,#4059,#4060,#4061,#4062,#4063,#4064,
#4065,#4066,#4067,#4068,#4069,#4070,#4071,#4072,#4073,#4074,#4075,#4076,
#4077,#4078,#4079,#4080,#4081,#4082),.UNSPECIFIED.,.F.,.F.,(4,2,2,2,2,2,
2,2,2,2,2,2,2,2,2,2,2,4),(-9.45989242392903,-9.43999077650971,-9.36038187512455,
-9.28427999581966,-9.20531546624748,-9.12662757343301,-9.04702763321718,
-8.96941790488596,-8.89241104834552,-8.81268983345869,-8.73597722731793,
-8.65647973487902,-8.5778031757691,-8.5018188310753,-8.42223856028909,-8.34442217750091,
-8.26778576297144,-8.19874268237018),.UNSPECIFIED.);
#80=B_SPLINE_CURVE_WITH_KNOTS('',3,(#4083,#4084,#4085,#4086,#4087,#4088,
#4089,#4090,#4091,#4092,#4093,#4094,#4095,#4096,#4097,#4098,#4099,#4100,
#4101,#4102,#4103,#4104,#4105,#4106,#4107,#4108,#4109,#4110,#4111,#4112,
#4113,#4114,#4115,#4116,#4117,#4118,#4119,#4120),.UNSPECIFIED.,.F.,.F.,
(4,2,2,2,2,2,2,2,2,2,2,2,2,2,2,2,2,2,4),(-8.21851276396746,-8.21373558189498,
-8.13386834694535,-8.05755710295663,-7.97892605602102,-7.89908098113983,
-7.81919898031824,-7.74071772777192,-7.66417313720762,-7.58350912693979,
-7.50592987918485,-7.42778926135171,-7.34813866162646,-7.27147276625184,
-7.19163483030402,-7.11303172035878,-7.03671511852042,-6.95685331088016,
-6.95266604471072),.UNSPECIFIED.);
#81=B_SPLINE_CURVE_WITH_KNOTS('',3,(#4125,#4126,#4127,#4128,#4129,#4130,
#4131,#4132,#4133,#4134,#4135,#4136,#4137,#4138,#4139,#4140,#4141,#4142,
#4143,#4144,#4145,#4146,#4147,#4148,#4149,#4150,#4151,#4152,#4153,#4154,
#4155,#4156,#4157,#4158,#4159,#4160),.UNSPECIFIED.,.F.,.F.,(4,2,2,2,2,2,
2,2,2,2,2,2,2,2,2,2,2,4),(-10.7208831151999,-10.689909461682,-10.6096449748488,
-10.5331987333682,-10.4537678957129,-10.376358802264,-10.2990102493312,
-10.2194492767843,-10.143369370979,-10.0651520735019,-9.98562100504683,
-9.90932376044898,-9.83006115144956,-9.75195515827296,-9.67474235452267,
-9.59446715610431,-9.51810101957741,-9.45989242392903),.UNSPECIFIED.);
#82=B_SPLINE_CURVE_WITH_KNOTS('',3,(#4161,#4162,#4163,#4164,#4165,#4166,
#4167,#4168,#4169,#4170,#4171,#4172,#4173,#4174,#4175,#4176,#4177,#4178,
#4179,#4180,#4181,#4182,#4183,#4184,#4185,#4186,#4187,#4188,#4189,#4190,
#4191,#4192,#4193,#4194,#4195,#4196),.UNSPECIFIED.,.F.,.F.,(4,2,2,2,2,2,
2,2,2,2,2,2,2,2,2,2,2,4),(-6.95266604471072,-6.87912035870533,-6.80161111519335,
-6.72177597678322,-6.64494587478012,-6.56472359442252,-6.48595176267986,
-6.40974122844908,-6.32992356240856,-6.25201727672208,-6.17494198405241,
-6.09490861806319,-6.0179008787191,-5.93846147131654,-5.8594675035079,-5.78324336357049,
-5.70343001040883,-5.6879113601691),.UNSPECIFIED.);
#83=B_SPLINE_CURVE_WITH_KNOTS('',3,(#4201,#4202,#4203,#4204,#4205,#4206,
#4207,#4208,#4209,#4210,#4211,#4212,#4213,#4214,#4215,#4216,#4217,#4218,
#4219,#4220,#4221,#4222,#4223,#4224,#4225,#4226,#4227,#4228,#4229,#4230,
#4231,#4232,#4233,#4234,#4235,#4236),.UNSPECIFIED.,.F.,.F.,(4,2,2,2,2,2,
2,2,2,2,2,2,2,2,2,2,2,4),(-11.9803245766439,-11.9373167530931,-11.8585934618904,
-11.7817902230109,-11.7019611013535,-11.6253997279527,-11.5477023803251,
-11.4682254817359,-11.3923417429942,-11.3137849692748,-11.2343306742371,
-11.1577318698951,-11.0781299881721,-11.0011901691327,-10.9236951007982,
-10.8441954672365,-10.7682685365538,-10.7208831151999),.UNSPECIFIED.);
#84=B_SPLINE_CURVE_WITH_KNOTS('',3,(#4237,#4238,#4239,#4240,#4241,#4242,
#4243,#4244,#4245,#4246,#4247,#4248,#4249,#4250,#4251,#4252,#4253,#4254,
#4255,#4256,#4257,#4258,#4259,#4260,#4261,#4262,#4263,#4264,#4265,#4266,
#4267,#4268,#4269,#4270,#4271,#4272),.UNSPECIFIED.,.F.,.F.,(4,2,2,2,2,2,
2,2,2,2,2,2,2,2,2,2,2,4),(-5.6879113601691,-5.62529684161333,-5.54854901162185,
-5.46826362292143,-5.39102857977524,-5.31227247591972,-5.23300989841653,
-5.15664034154526,-5.07678848006062,-4.99838116103412,-4.92183166154852,
-4.84124685797192,-4.7637405229502,-4.68553143909071,-4.6059606559999,-4.52936949203966,
-4.44957633005152,-4.42251287828457),.UNSPECIFIED.);
#85=B_SPLINE_CURVE_WITH_KNOTS('',3,(#4277,#4278,#4279,#4280,#4281,#4282,
#4283,#4284,#4285,#4286,#4287,#4288,#4289,#4290,#4291,#4292,#4293,#4294,
#4295,#4296,#4297,#4298,#4299,#4300,#4301,#4302,#4303,#4304,#4305,#4306,
#4307,#4308,#4309,#4310,#4311,#4312),.UNSPECIFIED.,.F.,.F.,(4,2,2,2,2,2,
2,2,2,2,2,2,2,2,2,2,2,4),(-13.2409568636929,-13.1857973798113,-13.1081455092838,
-13.0307997538635,-12.9503721070074,-12.8741918218951,-12.795946314629,
-12.7163879250462,-12.6402039653457,-12.561110295691,-12.4829974573744,
-12.4059433851361,-12.3258368643218,-12.249533657225,-12.1715840064512,
-12.0920886845932,-12.0161207543943,-11.9803245766439),.UNSPECIFIED.);
#86=B_SPLINE_CURVE_WITH_KNOTS('',3,(#4313,#4314,#4315,#4316,#4317,#4318,
#4319,#4320,#4321,#4322,#4323,#4324,#4325,#4326,#4327,#4328,#4329,#4330,
#4331,#4332,#4333,#4334,#4335,#4336,#4337,#4338,#4339,#4340,#4341,#4342,
#4343,#4344,#4345,#4346,#4347,#4348),.UNSPECIFIED.,.F.,.F.,(4,2,2,2,2,2,
2,2,2,2,2,2,2,2,2,2,2,4),(-4.42251287828457,-4.37105308848007,-4.29475658676344,
-4.2149367917279,-4.13728403482588,-4.05973519783431,-3.97998642459269,
-3.90323717095959,-3.82291167517872,-3.74423079741854,-3.66806093761842,
-3.58829265274099,-3.510477602882,-3.43337898390597,-3.35344313544485,-3.27652653462792,
-3.19699748173497,-3.15840542960694),.UNSPECIFIED.);
#87=B_SPLINE_CURVE_WITH_KNOTS('',3,(#4353,#4354,#4355,#4356,#4357,#4358,
#4359,#4360,#4361,#4362,#4363,#4364,#4365,#4366,#4367,#4368,#4369,#4370,
#4371,#4372,#4373,#4374,#4375,#4376,#4377,#4378,#4379,#4380,#4381,#4382,
#4383,#4384,#4385,#4386,#4387,#4388),.UNSPECIFIED.,.F.,.F.,(4,2,2,2,2,2,
2,2,2,2,2,2,2,2,2,2,2,4),(-14.5013677613806,-14.4340143197835,-14.357337425761,
-14.2796345736176,-14.2001052468701,-14.1241738883576,-14.0456101277613,
-13.9659484009548,-13.8893350084197,-13.8097206417991,-13.7326441155937,
-13.6551329843342,-13.5755730503643,-13.4995748837262,-13.4211982788963,
-13.3416565958452,-13.2652169977317,-13.2409568636929),.UNSPECIFIED.);
#88=B_SPLINE_CURVE_WITH_KNOTS('',3,(#4389,#4390,#4391,#4392,#4393,#4394,
#4395,#4396,#4397,#4398,#4399,#4400,#4401,#4402,#4403,#4404,#4405,#4406,
#4407,#4408,#4409,#4410,#4411,#4412,#4413,#4414,#4415,#4416,#4417,#4418,
#4419,#4420,#4421,#4422,#4423,#4424),.UNSPECIFIED.,.F.,.F.,(4,2,2,2,2,2,
2,2,2,2,2,2,2,2,2,2,2,4),(-3.15840542960694,-3.11810438438716,-3.04194530523324,
-2.96218919644079,-2.88415726256218,-2.80740869673208,-2.72723086835948,
-2.6500962409616,-2.5712724087441,-2.49211926891882,-2.41584052292748,-2.33605445076877,
-2.25775714016015,-2.18123275125624,-2.10076432831839,-2.02336662577393,
-1.94511786786739,-1.89413067066974),.UNSPECIFIED.);
#89=B_SPLINE_CURVE_WITH_KNOTS('',3,(#4429,#4430,#4431,#4432,#4433,#4434,
#4435,#4436,#4437,#4438,#4439,#4440,#4441,#4442,#4443,#4444,#4445,#4446,
#4447,#4448,#4449,#4450,#4451,#4452,#4453,#4454,#4455,#4456,#4457,#4458,
#4459,#4460,#4461,#4462,#4463,#4464),.UNSPECIFIED.,.F.,.F.,(4,2,2,2,2,2,
2,2,2,2,2,2,2,2,2,2,2,4),(-15.7622091439389,-15.6829898523921,-15.6067471990204,
-15.528513438186,-15.4489202057025,-15.3727404748348,-15.2936566676599,
-15.2153833658689,-15.1383330993407,-15.0582339695481,-14.9818408052142,
-14.9038949284596,-14.8243556056916,-14.7483661771305,-14.6695643193714,
-14.5906533835512,-14.5138453351592,-14.5013677613806),.UNSPECIFIED.);
#90=B_SPLINE_CURVE_WITH_KNOTS('',3,(#4465,#4466,#4467,#4468,#4469,#4470,
#4471,#4472,#4473,#4474,#4475,#4476,#4477,#4478,#4479,#4480,#4481,#4482,
#4483,#4484,#4485,#4486,#4487,#4488,#4489,#4490,#4491,#4492,#4493,#4494,
#4495,#4496,#4497,#4498,#4499,#4500),.UNSPECIFIED.,.F.,.F.,(4,2,2,2,2,2,
2,2,2,2,2,2,2,2,2,2,2,4),(-1.89413067066974,-1.86566387854342,-1.78918302276564,
-1.70947059360041,-1.63106398788885,-1.55481869217121,-1.47507701580335,
-1.39754087768896,-1.31998180733374,-1.24035706054127,-1.16372486431469,
-1.08332395037665,-1.00477168783817,-0.928673722312505,-0.848991237615832,
-0.771304718998596,-0.694211484813285,-0.631073530473631),.UNSPECIFIED.);
#91=B_SPLINE_CURVE_WITH_KNOTS('',3,(#4508,#4509,#4510,#4511,#4512,#4513,
#4514,#4515,#4516,#4517),.UNSPECIFIED.,.F.,.F.,(4,3,3,4),(0.0186025420886609,
0.399443095780039,0.791951766276959,0.961843099180382),.UNSPECIFIED.);
#92=B_SPLINE_CURVE_WITH_KNOTS('',3,(#4519,#4520,#4521,#4522,#4523,#4524,
#4525,#4526,#4527,#4528,#4529,#4530,#4531,#4532,#4533,#4534,#4535,#4536),
 .UNSPECIFIED.,.F.,.F.,(4,2,2,2,2,2,2,2,4),(-0.376269306197457,-0.343624542177792,
-0.312421269965175,-0.25987291948725,-0.205012849988066,-0.153112595643002,
-0.0910243275886042,-0.0438944746831949,-1.00000008707024E-6),
 .UNSPECIFIED.);
#93=B_SPLINE_CURVE_WITH_KNOTS('',3,(#4538,#4539,#4540,#4541,#4542,#4543,
#4544,#4545,#4546,#4547,#4548,#4549,#4550,#4551,#4552,#4553,#4554,#4555),
 .UNSPECIFIED.,.F.,.F.,(4,2,2,2,2,2,2,2,4),(-1.05438675280514,-0.870346440875757,
-0.698872384787591,-0.518061896275986,-0.346276386875803,-0.22927416645259,
-0.145876888593318,-0.0688156210803101,0.),.UNSPECIFIED.);
#94=B_SPLINE_CURVE_WITH_KNOTS('',3,(#4563,#4564,#4565,#4566,#4567,#4568,
#4569,#4570,#4571,#4572,#4573,#4574),.UNSPECIFIED.,.F.,.F.,(4,2,2,2,2,4),
(-0.313836142992068,-0.25677177702737,-0.19781608691674,-0.113507480641476,
-0.0353872570075592,-0.0260648083918944),.UNSPECIFIED.);
#95=B_SPLINE_CURVE_WITH_KNOTS('',3,(#4589,#4590,#4591,#4592),
 .UNSPECIFIED.,.F.,.F.,(4,4),(-0.0260648083918944,0.),.UNSPECIFIED.);
#96=B_SPLINE_CURVE_WITH_KNOTS('',3,(#4596,#4597,#4598,#4599,#4600,#4601,
#4602,#4603,#4604,#4605,#4606,#4607,#4608,#4609,#4610,#4611,#4612,#4613,
#4614,#4615),.UNSPECIFIED.,.F.,.F.,(4,2,2,2,2,2,2,2,2,4),(-0.631073530473631,
-0.61441175547036,-0.53762346866716,-0.458031245779653,-0.379277736775302,
-0.303215824772569,-0.223553831976816,-0.145661463287594,-0.0741741268612384,
-1.00000013547596E-6),.UNSPECIFIED.);
#97=B_SPLINE_CURVE_WITH_KNOTS('',3,(#4616,#4617,#4618,#4619,#4620,#4621),
 .UNSPECIFIED.,.F.,.F.,(4,2,4),(-0.113972621579486,-0.0620619568776889,
-0.000408441533670647),.UNSPECIFIED.);
#98=B_SPLINE_CURVE_WITH_KNOTS('',3,(#4622,#4623,#4624,#4625,#4626,#4627,
#4628,#4629,#4630,#4631,#4632,#4633,#4634,#4635,#4636,#4637,#4638,#4639,
#4640,#4641),.UNSPECIFIED.,.F.,.F.,(4,2,2,2,2,2,2,2,2,4),(-16.3669314512571,
-16.2989761330899,-16.2322666274892,-16.1539071068032,-16.0743459352974,
-15.997920071627,-15.9185170450843,-15.8407363969791,-15.7634021047055,
-15.7622091439389),.UNSPECIFIED.);
#99=B_SPLINE_CURVE_WITH_KNOTS('',3,(#7184,#7185,#7186,#7187,#7188,#7189,
#7190,#7191,#7192,#7193,#7194,#7195,#7196,#7197,#7198,#7199,#7200,#7201),
 .UNSPECIFIED.,.F.,.F.,(4,2,2,2,2,2,2,2,4),(0.,0.000446496312049465,0.00089299262409893,
0.00133948893614839,0.00178598524819786,0.00223248156024732,0.00267897787229679,
0.00312547418434625,0.00357196805342217),.UNSPECIFIED.);
#100=B_SPLINE_CURVE_WITH_KNOTS('',3,(#9769,#9770,#9771,#9772,#9773,#9774,
#9775,#9776,#9777,#9778,#9779,#9780,#9781,#9782,#9783,#9784),
 .UNSPECIFIED.,.F.,.F.,(4,2,2,2,2,2,2,4),(2.04424781819707E-8,0.000444285842515272,
0.000888571685030545,0.00177714337006109,0.00222142921257636,0.00266571505509163,
0.00311000089760691,0.00355428674012218),.UNSPECIFIED.);
#101=(
BOUNDED_CURVE()
B_SPLINE_CURVE(2,(#3153,#3154,#3155,#3156,#3157,#3158,#3159,#3160,#3161,
#3162,#3163),.UNSPECIFIED.,.F.,.F.)
B_SPLINE_CURVE_WITH_KNOTS((3,2,2,2,2,3),(0.839018811586759,0.840309935413827,
0.84188650189678,0.843463068379733,0.845039634862686,0.846616201345638),
 .UNSPECIFIED.)
CURVE()
GEOMETRIC_REPRESENTATION_ITEM()
RATIONAL_B_SPLINE_CURVE((0.960270358787523,0.89028195431901,1.,0.866025403784439,
1.,0.866025403784439,1.,0.866025403784439,1.,0.866025403784439,1.))
REPRESENTATION_ITEM('')
);
#102=(
BOUNDED_CURVE()
B_SPLINE_CURVE(2,(#3166,#3167,#3168,#3169,#3170,#3171,#3172,#3173,#3174),
 .UNSPECIFIED.,.F.,.F.)
B_SPLINE_CURVE_WITH_KNOTS((3,2,2,2,3),(0.839084484051456,0.839622641509434,
0.841194968553459,0.842767295597484,0.844339622641509),.UNSPECIFIED.)
CURVE()
GEOMETRIC_REPRESENTATION_ITEM()
RATIONAL_B_SPLINE_CURVE((0.939679100585349,0.954144763707433,1.,0.866025403784439,
1.,0.866025403784439,1.,0.866025403784439,1.))
REPRESENTATION_ITEM('')
);
#103=(
BOUNDED_CURVE()
B_SPLINE_CURVE(2,(#3179,#3180,#3181,#3182,#3183,#3184,#3185,#3186,#3187,
#3188,#3189,#3190,#3191),.UNSPECIFIED.,.F.,.F.)
B_SPLINE_CURVE_WITH_KNOTS((3,2,2,2,2,2,3),(0.846616201345638,0.848192767828591,
0.849769334311544,0.851345900794497,0.852922467277449,0.854499033760402,
0.856075600243355),.UNSPECIFIED.)
CURVE()
GEOMETRIC_REPRESENTATION_ITEM()
RATIONAL_B_SPLINE_CURVE((1.,0.866025403784439,1.,0.866025403784439,1.,0.866025403784439,
1.,0.866025403784439,1.,0.866025403784439,1.,0.866025403784439,1.))
REPRESENTATION_ITEM('')
);
#104=(
BOUNDED_CURVE()
B_SPLINE_CURVE(2,(#3192,#3193,#3194,#3195,#3196,#3197,#3198,#3199,#3200,
#3201,#3202,#3203,#3204),.UNSPECIFIED.,.F.,.F.)
B_SPLINE_CURVE_WITH_KNOTS((3,2,2,2,2,2,3),(0.844339622641509,0.845911949685535,
0.84748427672956,0.849056603773585,0.85062893081761,0.852201257861635,0.85377358490566),
 .UNSPECIFIED.)
CURVE()
GEOMETRIC_REPRESENTATION_ITEM()
RATIONAL_B_SPLINE_CURVE((1.,0.866025403784439,1.,0.866025403784439,1.,0.866025403784439,
1.,0.866025403784439,1.,0.866025403784439,1.,0.866025403784439,1.))
REPRESENTATION_ITEM('')
);
#105=(
BOUNDED_CURVE()
B_SPLINE_CURVE(2,(#3209,#3210,#3211,#3212,#3213,#3214,#3215,#3216,#3217,
#3218,#3219,#3220,#3221),.UNSPECIFIED.,.F.,.F.)
B_SPLINE_CURVE_WITH_KNOTS((3,2,2,2,2,2,3),(0.856075600243355,0.857652166726308,
0.85922873320926,0.860805299692213,0.862381866175166,0.863958432658119,
0.865534999141071),.UNSPECIFIED.)
CURVE()
GEOMETRIC_REPRESENTATION_ITEM()
RATIONAL_B_SPLINE_CURVE((1.,0.866025403784439,1.,0.866025403784439,1.,0.866025403784439,
1.,0.866025403784439,1.,0.866025403784439,1.,0.866025403784439,1.))
REPRESENTATION_ITEM('')
);
#106=(
BOUNDED_CURVE()
B_SPLINE_CURVE(2,(#3222,#3223,#3224,#3225,#3226,#3227,#3228,#3229,#3230,
#3231,#3232,#3233,#3234),.UNSPECIFIED.,.F.,.F.)
B_SPLINE_CURVE_WITH_KNOTS((3,2,2,2,2,2,3),(0.85377358490566,0.855345911949686,
0.856918238993711,0.858490566037736,0.860062893081761,0.861635220125786,
0.863207547169811),.UNSPECIFIED.)
CURVE()
GEOMETRIC_REPRESENTATION_ITEM()
RATIONAL_B_SPLINE_CURVE((1.,0.866025403784439,1.,0.866025403784439,1.,0.866025403784439,
1.,0.866025403784439,1.,0.866025403784439,1.,0.866025403784439,1.))
REPRESENTATION_ITEM('')
);
#107=(
BOUNDED_CURVE()
B_SPLINE_CURVE(2,(#3239,#3240,#3241,#3242,#3243,#3244,#3245,#3246,#3247,
#3248,#3249,#3250,#3251),.UNSPECIFIED.,.F.,.F.)
B_SPLINE_CURVE_WITH_KNOTS((3,2,2,2,2,2,3),(0.865534999141071,0.867111565624024,
0.868688132106977,0.87026469858993,0.871841265072883,0.873417831555835,
0.874994398038788),.UNSPECIFIED.)
CURVE()
GEOMETRIC_REPRESENTATION_ITEM()
RATIONAL_B_SPLINE_CURVE((1.,0.866025403784439,1.,0.866025403784439,1.,0.866025403784439,
1.,0.866025403784439,1.,0.866025403784439,1.,0.866025403784439,1.))
REPRESENTATION_ITEM('')
);
#108=(
BOUNDED_CURVE()
B_SPLINE_CURVE(2,(#3252,#3253,#3254,#3255,#3256,#3257,#3258,#3259,#3260,
#3261,#3262,#3263,#3264),.UNSPECIFIED.,.F.,.F.)
B_SPLINE_CURVE_WITH_KNOTS((3,2,2,2,2,2,3),(0.863207547169811,0.864779874213837,
0.866352201257862,0.867924528301887,0.869496855345912,0.871069182389937,
0.872641509433962),.UNSPECIFIED.)
CURVE()
GEOMETRIC_REPRESENTATION_ITEM()
RATIONAL_B_SPLINE_CURVE((1.,0.866025403784439,1.,0.866025403784439,1.,0.866025403784439,
1.,0.866025403784439,1.,0.866025403784439,1.,0.866025403784439,1.))
REPRESENTATION_ITEM('')
);
#109=(
BOUNDED_CURVE()
B_SPLINE_CURVE(2,(#3269,#3270,#3271,#3272,#3273,#3274,#3275,#3276,#3277,
#3278,#3279,#3280,#3281),.UNSPECIFIED.,.F.,.F.)
B_SPLINE_CURVE_WITH_KNOTS((3,2,2,2,2,2,3),(0.874994398038788,0.876570964521741,
0.878147531004694,0.879724097487646,0.881300663970599,0.882877230453552,
0.884453796936505),.UNSPECIFIED.)
CURVE()
GEOMETRIC_REPRESENTATION_ITEM()
RATIONAL_B_SPLINE_CURVE((1.,0.866025403784439,1.,0.866025403784439,1.,0.866025403784439,
1.,0.866025403784439,1.,0.866025403784439,1.,0.866025403784439,1.))
REPRESENTATION_ITEM('')
);
#110=(
BOUNDED_CURVE()
B_SPLINE_CURVE(2,(#3282,#3283,#3284,#3285,#3286,#3287,#3288,#3289,#3290,
#3291,#3292,#3293,#3294),.UNSPECIFIED.,.F.,.F.)
B_SPLINE_CURVE_WITH_KNOTS((3,2,2,2,2,2,3),(0.872641509433962,0.874213836477987,
0.875786163522013,0.877358490566038,0.878930817610063,0.880503144654088,
0.882075471698113),.UNSPECIFIED.)
CURVE()
GEOMETRIC_REPRESENTATION_ITEM()
RATIONAL_B_SPLINE_CURVE((1.,0.866025403784439,1.,0.866025403784439,1.,0.866025403784439,
1.,0.866025403784439,1.,0.866025403784439,1.,0.866025403784439,1.))
REPRESENTATION_ITEM('')
);
#111=(
BOUNDED_CURVE()
B_SPLINE_CURVE(2,(#3299,#3300,#3301,#3302,#3303,#3304,#3305,#3306,#3307,
#3308,#3309,#3310,#3311),.UNSPECIFIED.,.F.,.F.)
B_SPLINE_CURVE_WITH_KNOTS((3,2,2,2,2,2,3),(0.884453796936505,0.886030363419458,
0.88760692990241,0.889183496385363,0.890760062868316,0.892336629351269,
0.893913195834221),.UNSPECIFIED.)
CURVE()
GEOMETRIC_REPRESENTATION_ITEM()
RATIONAL_B_SPLINE_CURVE((1.,0.866025403784439,1.,0.866025403784439,1.,0.866025403784439,
1.,0.866025403784439,1.,0.866025403784439,1.,0.866025403784439,1.))
REPRESENTATION_ITEM('')
);
#112=(
BOUNDED_CURVE()
B_SPLINE_CURVE(2,(#3312,#3313,#3314,#3315,#3316,#3317,#3318,#3319,#3320,
#3321,#3322,#3323,#3324),.UNSPECIFIED.,.F.,.F.)
B_SPLINE_CURVE_WITH_KNOTS((3,2,2,2,2,2,3),(0.882075471698113,0.883647798742138,
0.885220125786163,0.886792452830189,0.888364779874214,0.889937106918239,
0.891509433962264),.UNSPECIFIED.)
CURVE()
GEOMETRIC_REPRESENTATION_ITEM()
RATIONAL_B_SPLINE_CURVE((1.,0.866025403784439,1.,0.866025403784439,1.,0.866025403784439,
1.,0.866025403784439,1.,0.866025403784439,1.,0.866025403784439,1.))
REPRESENTATION_ITEM('')
);
#113=(
BOUNDED_CURVE()
B_SPLINE_CURVE(2,(#3329,#3330,#3331,#3332,#3333,#3334,#3335,#3336,#3337,
#3338,#3339,#3340,#3341),.UNSPECIFIED.,.F.,.F.)
B_SPLINE_CURVE_WITH_KNOTS((3,2,2,2,2,2,3),(0.893913195834221,0.895489762317174,
0.897066328800127,0.89864289528308,0.900219461766032,0.901796028248985,
0.903372594731938),.UNSPECIFIED.)
CURVE()
GEOMETRIC_REPRESENTATION_ITEM()
RATIONAL_B_SPLINE_CURVE((1.,0.866025403784439,1.,0.866025403784439,1.,0.866025403784439,
1.,0.866025403784439,1.,0.866025403784439,1.,0.866025403784439,1.))
REPRESENTATION_ITEM('')
);
#114=(
BOUNDED_CURVE()
B_SPLINE_CURVE(2,(#3342,#3343,#3344,#3345,#3346,#3347,#3348,#3349,#3350,
#3351,#3352,#3353,#3354),.UNSPECIFIED.,.F.,.F.)
B_SPLINE_CURVE_WITH_KNOTS((3,2,2,2,2,2,3),(0.891509433962264,0.893081761006289,
0.894654088050314,0.89622641509434,0.897798742138365,0.89937106918239,0.900943396226415),
 .UNSPECIFIED.)
CURVE()
GEOMETRIC_REPRESENTATION_ITEM()
RATIONAL_B_SPLINE_CURVE((1.,0.866025403784439,1.,0.866025403784439,1.,0.866025403784439,
1.,0.866025403784439,1.,0.866025403784439,1.,0.866025403784439,1.))
REPRESENTATION_ITEM('')
);
#115=(
BOUNDED_CURVE()
B_SPLINE_CURVE(2,(#3359,#3360,#3361,#3362,#3363,#3364,#3365,#3366,#3367,
#3368,#3369,#3370,#3371),.UNSPECIFIED.,.F.,.F.)
B_SPLINE_CURVE_WITH_KNOTS((3,2,2,2,2,2,3),(0.903372594731938,0.904949161214891,
0.906525727697844,0.908102294180796,0.909678860663749,0.911255427146702,
0.912831993629655),.UNSPECIFIED.)
CURVE()
GEOMETRIC_REPRESENTATION_ITEM()
RATIONAL_B_SPLINE_CURVE((1.,0.866025403784439,1.,0.866025403784439,1.,0.866025403784439,
1.,0.866025403784439,1.,0.866025403784439,1.,0.866025403784439,1.))
REPRESENTATION_ITEM('')
);
#116=(
BOUNDED_CURVE()
B_SPLINE_CURVE(2,(#3372,#3373,#3374,#3375,#3376,#3377,#3378,#3379,#3380,
#3381,#3382,#3383,#3384),.UNSPECIFIED.,.F.,.F.)
B_SPLINE_CURVE_WITH_KNOTS((3,2,2,2,2,2,3),(0.900943396226415,0.90251572327044,
0.904088050314465,0.905660377358491,0.907232704402516,0.908805031446541,
0.910377358490566),.UNSPECIFIED.)
CURVE()
GEOMETRIC_REPRESENTATION_ITEM()
RATIONAL_B_SPLINE_CURVE((1.,0.866025403784439,1.,0.866025403784439,1.,0.866025403784439,
1.,0.866025403784439,1.,0.866025403784439,1.,0.866025403784439,1.))
REPRESENTATION_ITEM('')
);
#117=(
BOUNDED_CURVE()
B_SPLINE_CURVE(2,(#3389,#3390,#3391,#3392,#3393,#3394,#3395,#3396,#3397,
#3398,#3399,#3400,#3401),.UNSPECIFIED.,.F.,.F.)
B_SPLINE_CURVE_WITH_KNOTS((3,2,2,2,2,2,3),(0.912831993629655,0.914408560112607,
0.91598512659556,0.917561693078513,0.919138259561466,0.920714826044419,
0.922291392527371),.UNSPECIFIED.)
CURVE()
GEOMETRIC_REPRESENTATION_ITEM()
RATIONAL_B_SPLINE_CURVE((1.,0.866025403784439,1.,0.866025403784439,1.,0.866025403784439,
1.,0.866025403784439,1.,0.866025403784439,1.,0.866025403784439,1.))
REPRESENTATION_ITEM('')
);
#118=(
BOUNDED_CURVE()
B_SPLINE_CURVE(2,(#3402,#3403,#3404,#3405,#3406,#3407,#3408,#3409,#3410,
#3411,#3412,#3413,#3414),.UNSPECIFIED.,.F.,.F.)
B_SPLINE_CURVE_WITH_KNOTS((3,2,2,2,2,2,3),(0.910377358490566,0.911949685534591,
0.913522012578616,0.915094339622642,0.916666666666667,0.918238993710692,
0.919811320754717),.UNSPECIFIED.)
CURVE()
GEOMETRIC_REPRESENTATION_ITEM()
RATIONAL_B_SPLINE_CURVE((1.,0.866025403784439,1.,0.866025403784439,1.,0.866025403784439,
1.,0.866025403784439,1.,0.866025403784439,1.,0.866025403784439,1.))
REPRESENTATION_ITEM('')
);
#119=(
BOUNDED_CURVE()
B_SPLINE_CURVE(2,(#3419,#3420,#3421,#3422,#3423,#3424,#3425,#3426,#3427,
#3428,#3429,#3430,#3431),.UNSPECIFIED.,.F.,.F.)
B_SPLINE_CURVE_WITH_KNOTS((3,2,2,2,2,2,3),(0.922291392527371,0.923867959010324,
0.925444525493277,0.92702109197623,0.928597658459182,0.930174224942135,
0.931750791425088),.UNSPECIFIED.)
CURVE()
GEOMETRIC_REPRESENTATION_ITEM()
RATIONAL_B_SPLINE_CURVE((1.,0.866025403784439,1.,0.866025403784439,1.,0.866025403784439,
1.,0.866025403784439,1.,0.866025403784439,1.,0.866025403784439,1.))
REPRESENTATION_ITEM('')
);
#120=(
BOUNDED_CURVE()
B_SPLINE_CURVE(2,(#3432,#3433,#3434,#3435,#3436,#3437,#3438,#3439,#3440,
#3441,#3442,#3443,#3444),.UNSPECIFIED.,.F.,.F.)
B_SPLINE_CURVE_WITH_KNOTS((3,2,2,2,2,2,3),(0.919811320754717,0.921383647798742,
0.922955974842767,0.924528301886792,0.926100628930818,0.927672955974843,
0.929245283018868),.UNSPECIFIED.)
CURVE()
GEOMETRIC_REPRESENTATION_ITEM()
RATIONAL_B_SPLINE_CURVE((1.,0.866025403784439,1.,0.866025403784439,1.,0.866025403784439,
1.,0.866025403784439,1.,0.866025403784439,1.,0.866025403784439,1.))
REPRESENTATION_ITEM('')
);
#121=(
BOUNDED_CURVE()
B_SPLINE_CURVE(2,(#3449,#3450,#3451,#3452,#3453,#3454,#3455,#3456,#3457,
#3458,#3459,#3460,#3461),.UNSPECIFIED.,.F.,.F.)
B_SPLINE_CURVE_WITH_KNOTS((3,2,2,2,2,2,3),(0.931750791425088,0.933327357908041,
0.934903924390993,0.936480490873946,0.938057057356899,0.939633623839852,
0.941210190322805),.UNSPECIFIED.)
CURVE()
GEOMETRIC_REPRESENTATION_ITEM()
RATIONAL_B_SPLINE_CURVE((1.,0.866025403784439,1.,0.866025403784439,1.,0.866025403784439,
1.,0.866025403784439,1.,0.866025403784439,1.,0.866025403784439,1.))
REPRESENTATION_ITEM('')
);
#122=(
BOUNDED_CURVE()
B_SPLINE_CURVE(2,(#3462,#3463,#3464,#3465,#3466,#3467,#3468,#3469,#3470,
#3471,#3472,#3473,#3474),.UNSPECIFIED.,.F.,.F.)
B_SPLINE_CURVE_WITH_KNOTS((3,2,2,2,2,2,3),(0.929245283018868,0.930817610062893,
0.932389937106918,0.933962264150943,0.935534591194969,0.937106918238994,
0.938679245283019),.UNSPECIFIED.)
CURVE()
GEOMETRIC_REPRESENTATION_ITEM()
RATIONAL_B_SPLINE_CURVE((1.,0.866025403784439,1.,0.866025403784439,1.,0.866025403784439,
1.,0.866025403784439,1.,0.866025403784439,1.,0.866025403784439,1.))
REPRESENTATION_ITEM('')
);
#123=(
BOUNDED_CURVE()
B_SPLINE_CURVE(2,(#3479,#3480,#3481,#3482,#3483,#3484,#3485,#3486,#3487,
#3488,#3489,#3490,#3491),.UNSPECIFIED.,.F.,.F.)
B_SPLINE_CURVE_WITH_KNOTS((3,2,2,2,2,2,3),(0.941210190322805,0.942786756805757,
0.94436332328871,0.945939889771663,0.947516456254616,0.949093022737568,
0.950669589220521),.UNSPECIFIED.)
CURVE()
GEOMETRIC_REPRESENTATION_ITEM()
RATIONAL_B_SPLINE_CURVE((1.,0.866025403784439,1.,0.866025403784439,1.,0.866025403784439,
1.,0.866025403784439,1.,0.866025403784439,1.,0.866025403784439,1.))
REPRESENTATION_ITEM('')
);
#124=(
BOUNDED_CURVE()
B_SPLINE_CURVE(2,(#3492,#3493,#3494,#3495,#3496,#3497,#3498,#3499,#3500,
#3501,#3502,#3503,#3504),.UNSPECIFIED.,.F.,.F.)
B_SPLINE_CURVE_WITH_KNOTS((3,2,2,2,2,2,3),(0.938679245283019,0.940251572327044,
0.941823899371069,0.943396226415094,0.944968553459119,0.946540880503145,
0.94811320754717),.UNSPECIFIED.)
CURVE()
GEOMETRIC_REPRESENTATION_ITEM()
RATIONAL_B_SPLINE_CURVE((1.,0.866025403784439,1.,0.866025403784439,1.,0.866025403784439,
1.,0.866025403784439,1.,0.866025403784439,1.,0.866025403784439,1.))
REPRESENTATION_ITEM('')
);
#125=(
BOUNDED_CURVE()
B_SPLINE_CURVE(2,(#3509,#3510,#3511,#3512,#3513,#3514,#3515,#3516,#3517,
#3518,#3519,#3520,#3521),.UNSPECIFIED.,.F.,.F.)
B_SPLINE_CURVE_WITH_KNOTS((3,2,2,2,2,2,3),(0.950669589220521,0.952246155703474,
0.953822722186427,0.95539928866938,0.956975855152332,0.958552421635285,
0.960128988118238),.UNSPECIFIED.)
CURVE()
GEOMETRIC_REPRESENTATION_ITEM()
RATIONAL_B_SPLINE_CURVE((1.,0.866025403784439,1.,0.866025403784439,1.,0.866025403784439,
1.,0.866025403784439,1.,0.866025403784439,1.,0.866025403784439,1.))
REPRESENTATION_ITEM('')
);
#126=(
BOUNDED_CURVE()
B_SPLINE_CURVE(2,(#3522,#3523,#3524,#3525,#3526,#3527,#3528,#3529,#3530,
#3531,#3532,#3533,#3534),.UNSPECIFIED.,.F.,.F.)
B_SPLINE_CURVE_WITH_KNOTS((3,2,2,2,2,2,3),(0.94811320754717,0.949685534591195,
0.95125786163522,0.952830188679245,0.95440251572327,0.955974842767296,0.957547169811321),
 .UNSPECIFIED.)
CURVE()
GEOMETRIC_REPRESENTATION_ITEM()
RATIONAL_B_SPLINE_CURVE((1.,0.866025403784439,1.,0.866025403784439,1.,0.866025403784439,
1.,0.866025403784439,1.,0.866025403784439,1.,0.866025403784439,1.))
REPRESENTATION_ITEM('')
);
#127=(
BOUNDED_CURVE()
B_SPLINE_CURVE(2,(#7202,#7203,#7204,#7205,#7206,#7207,#7208,#7209,#7210,
#7211,#7212,#7213,#7214),.UNSPECIFIED.,.F.,.F.)
B_SPLINE_CURVE_WITH_KNOTS((3,2,2,2,2,2,3),(0.957547169811321,0.959119496855346,
0.960691823899371,0.962264150943396,0.963836477987421,0.965408805031447,
0.9665584458795),.UNSPECIFIED.)
CURVE()
GEOMETRIC_REPRESENTATION_ITEM()
RATIONAL_B_SPLINE_CURVE((1.,0.866025403784439,1.,0.866025403784439,1.,0.866025403784439,
1.,0.866025403784439,1.,0.866025403784439,1.,0.902041582890659,0.947331986880629))
REPRESENTATION_ITEM('')
);
#128=(
BOUNDED_CURVE()
B_SPLINE_CURVE(2,(#7216,#7217,#7218,#7219,#7220,#7221,#7222,#7223,#7224,
#7225,#7226),.UNSPECIFIED.,.F.,.F.)
B_SPLINE_CURVE_WITH_KNOTS((3,2,2,2,2,3),(0.960128988118238,0.961705554601191,
0.963282121084143,0.964858687567096,0.966435254050049,0.966840628802582),
 .UNSPECIFIED.)
CURVE()
GEOMETRIC_REPRESENTATION_ITEM()
RATIONAL_B_SPLINE_CURVE((1.,0.866025403784439,1.,0.866025403784439,1.,0.866025403784439,
1.,0.866025403784439,1.,0.965551773823772,0.948818552136593))
REPRESENTATION_ITEM('')
);
#129=CONICAL_SURFACE('',#2171,40.283264100914,1.20427718387609);
#130=CONICAL_SURFACE('',#2172,40.283264100914,1.20427718387609);
#131=CONICAL_SURFACE('',#2266,2.01,0.785398163397453);
#132=CONICAL_SURFACE('',#2278,2.,0.78539816339745);
#133=CONICAL_SURFACE('',#2279,2.01,0.785398163397453);
#134=TOROIDAL_SURFACE('',#2118,6.,1.);
#135=TOROIDAL_SURFACE('',#2123,6.,1.);
#136=TOROIDAL_SURFACE('',#2142,41.0000000000046,2.);
#137=TOROIDAL_SURFACE('',#2150,16.0000000000046,2.);
#138=TOROIDAL_SURFACE('',#2159,15.9999999999978,2.);
#139=TOROIDAL_SURFACE('',#2162,33.9999999999978,2.);
#140=TOROIDAL_SURFACE('',#2180,34.0000000000017,2.);
#141=TOROIDAL_SURFACE('',#2271,2.4,0.4);
#142=TOROIDAL_SURFACE('',#2274,3.9385786437627,0.1);
#143=SHAPE_REPRESENTATION_RELATIONSHIP('SRR','None',#9938,#150);
#144=SHAPE_REPRESENTATION_RELATIONSHIP('SRR','None',#9939,#151);
#145=SHAPE_REPRESENTATION_RELATIONSHIP('SRR','None',#9940,#152);
#146=SHAPE_REPRESENTATION_RELATIONSHIP('SRR','None',#9941,#153);
#147=SHAPE_REPRESENTATION_RELATIONSHIP('SRR','None',#9942,#154);
#148=SHAPE_REPRESENTATION_RELATIONSHIP('SRR','None',#9943,#155);
#149=SHAPE_REPRESENTATION_RELATIONSHIP('SRR','None',#9944,#156);
#150=ADVANCED_BREP_SHAPE_REPRESENTATION('',(#164),#9896);
#151=ADVANCED_BREP_SHAPE_REPRESENTATION('',(#165),#9897);
#152=ADVANCED_BREP_SHAPE_REPRESENTATION('',(#166),#9898);
#153=ADVANCED_BREP_SHAPE_REPRESENTATION('',(#167),#9899);
#154=ADVANCED_BREP_SHAPE_REPRESENTATION('',(#168),#9900);
#155=ADVANCED_BREP_SHAPE_REPRESENTATION('',(#169),#9901);
#156=ADVANCED_BREP_SHAPE_REPRESENTATION('',(#170),#9902);
#157=STYLED_ITEM('',(#9982),#164);
#158=STYLED_ITEM('',(#9983),#165);
#159=STYLED_ITEM('',(#9982),#166);
#160=STYLED_ITEM('',(#9983),#167);
#161=STYLED_ITEM('',(#9982),#168);
#162=STYLED_ITEM('',(#9984),#169);
#163=STYLED_ITEM('',(#9985),#170);
#164=MANIFOLD_SOLID_BREP('Body1',#2022);
#165=MANIFOLD_SOLID_BREP('Body1',#2023);
#166=MANIFOLD_SOLID_BREP('Body1',#2024);
#167=MANIFOLD_SOLID_BREP('Body1',#2025);
#168=MANIFOLD_SOLID_BREP('Body1',#2026);
#169=MANIFOLD_SOLID_BREP('Body1',#2027);
#170=MANIFOLD_SOLID_BREP('Body1',#2028);
#171=FACE_BOUND('',#373,.T.);
#172=FACE_BOUND('',#375,.T.);
#173=FACE_BOUND('',#379,.T.);
#174=FACE_BOUND('',#380,.T.);
#175=FACE_BOUND('',#404,.T.);
#176=FACE_BOUND('',#406,.T.);
#177=FACE_BOUND('',#408,.T.);
#178=FACE_BOUND('',#410,.T.);
#179=FACE_BOUND('',#412,.T.);
#180=FACE_BOUND('',#414,.T.);
#181=FACE_BOUND('',#418,.T.);
#182=FACE_BOUND('',#420,.T.);
#183=FACE_BOUND('',#426,.T.);
#184=FACE_BOUND('',#427,.T.);
#185=FACE_BOUND('',#428,.T.);
#186=FACE_BOUND('',#430,.T.);
#187=FACE_BOUND('',#435,.T.);
#188=FACE_BOUND('',#436,.T.);
#189=FACE_BOUND('',#437,.T.);
#190=FACE_BOUND('',#441,.T.);
#191=FACE_BOUND('',#446,.T.);
#192=FACE_BOUND('',#447,.T.);
#193=FACE_BOUND('',#449,.T.);
#194=FACE_BOUND('',#450,.T.);
#195=FACE_BOUND('',#493,.T.);
#196=PLANE('',#2115);
#197=PLANE('',#2116);
#198=PLANE('',#2133);
#199=PLANE('',#2134);
#200=PLANE('',#2135);
#201=PLANE('',#2136);
#202=PLANE('',#2137);
#203=PLANE('',#2138);
#204=PLANE('',#2139);
#205=PLANE('',#2140);
#206=PLANE('',#2183);
#207=PLANE('',#2184);
#208=PLANE('',#2185);
#209=PLANE('',#2186);
#210=PLANE('',#2187);
#211=PLANE('',#2188);
#212=PLANE('',#2196);
#213=PLANE('',#2197);
#214=PLANE('',#2211);
#215=PLANE('',#2212);
#216=PLANE('',#2213);
#217=PLANE('',#2214);
#218=PLANE('',#2215);
#219=PLANE('',#2216);
#220=PLANE('',#2217);
#221=PLANE('',#2218);
#222=PLANE('',#2219);
#223=PLANE('',#2220);
#224=PLANE('',#2228);
#225=PLANE('',#2229);
#226=PLANE('',#2230);
#227=PLANE('',#2231);
#228=PLANE('',#2232);
#229=PLANE('',#2233);
#230=PLANE('',#2283);
#231=PLANE('',#2284);
#232=PLANE('',#2285);
#233=PLANE('',#2286);
#234=PLANE('',#2287);
#235=PLANE('',#2288);
#236=PLANE('',#2289);
#237=PLANE('',#2290);
#238=PLANE('',#2291);
#239=PLANE('',#2292);
#240=PLANE('',#2293);
#241=PLANE('',#2294);
#242=PLANE('',#2295);
#243=PLANE('',#2296);
#244=PLANE('',#2297);
#245=PLANE('',#2298);
#246=PLANE('',#2299);
#247=PLANE('',#2300);
#248=PLANE('',#2301);
#249=PLANE('',#2302);
#250=PLANE('',#2303);
#251=PLANE('',#2304);
#252=FACE_OUTER_BOUND('',#370,.T.);
#253=FACE_OUTER_BOUND('',#371,.T.);
#254=FACE_OUTER_BOUND('',#372,.T.);
#255=FACE_OUTER_BOUND('',#374,.T.);
#256=FACE_OUTER_BOUND('',#376,.T.);
#257=FACE_OUTER_BOUND('',#377,.T.);
#258=FACE_OUTER_BOUND('',#378,.T.);
#259=FACE_OUTER_BOUND('',#381,.T.);
#260=FACE_OUTER_BOUND('',#382,.T.);
#261=FACE_OUTER_BOUND('',#383,.T.);
#262=FACE_OUTER_BOUND('',#384,.T.);
#263=FACE_OUTER_BOUND('',#385,.T.);
#264=FACE_OUTER_BOUND('',#386,.T.);
#265=FACE_OUTER_BOUND('',#387,.T.);
#266=FACE_OUTER_BOUND('',#388,.T.);
#267=FACE_OUTER_BOUND('',#389,.T.);
#268=FACE_OUTER_BOUND('',#390,.T.);
#269=FACE_OUTER_BOUND('',#391,.T.);
#270=FACE_OUTER_BOUND('',#392,.T.);
#271=FACE_OUTER_BOUND('',#393,.T.);
#272=FACE_OUTER_BOUND('',#394,.T.);
#273=FACE_OUTER_BOUND('',#395,.T.);
#274=FACE_OUTER_BOUND('',#396,.T.);
#275=FACE_OUTER_BOUND('',#397,.T.);
#276=FACE_OUTER_BOUND('',#398,.T.);
#277=FACE_OUTER_BOUND('',#399,.T.);
#278=FACE_OUTER_BOUND('',#400,.T.);
#279=FACE_OUTER_BOUND('',#401,.T.);
#280=FACE_OUTER_BOUND('',#402,.T.);
#281=FACE_OUTER_BOUND('',#403,.T.);
#282=FACE_OUTER_BOUND('',#405,.T.);
#283=FACE_OUTER_BOUND('',#407,.T.);
#284=FACE_OUTER_BOUND('',#409,.T.);
#285=FACE_OUTER_BOUND('',#411,.T.);
#286=FACE_OUTER_BOUND('',#413,.T.);
#287=FACE_OUTER_BOUND('',#415,.T.);
#288=FACE_OUTER_BOUND('',#416,.T.);
#289=FACE_OUTER_BOUND('',#417,.T.);
#290=FACE_OUTER_BOUND('',#419,.T.);
#291=FACE_OUTER_BOUND('',#421,.T.);
#292=FACE_OUTER_BOUND('',#422,.T.);
#293=FACE_OUTER_BOUND('',#423,.T.);
#294=FACE_OUTER_BOUND('',#424,.T.);
#295=FACE_OUTER_BOUND('',#425,.T.);
#296=FACE_OUTER_BOUND('',#429,.T.);
#297=FACE_OUTER_BOUND('',#431,.T.);
#298=FACE_OUTER_BOUND('',#432,.T.);
#299=FACE_OUTER_BOUND('',#433,.T.);
#300=FACE_OUTER_BOUND('',#434,.T.);
#301=FACE_OUTER_BOUND('',#438,.T.);
#302=FACE_OUTER_BOUND('',#439,.T.);
#303=FACE_OUTER_BOUND('',#440,.T.);
#304=FACE_OUTER_BOUND('',#442,.T.);
#305=FACE_OUTER_BOUND('',#443,.T.);
#306=FACE_OUTER_BOUND('',#444,.T.);
#307=FACE_OUTER_BOUND('',#445,.T.);
#308=FACE_OUTER_BOUND('',#448,.T.);
#309=FACE_OUTER_BOUND('',#451,.T.);
#310=FACE_OUTER_BOUND('',#452,.T.);
#311=FACE_OUTER_BOUND('',#453,.T.);
#312=FACE_OUTER_BOUND('',#454,.T.);
#313=FACE_OUTER_BOUND('',#455,.T.);
#314=FACE_OUTER_BOUND('',#456,.T.);
#315=FACE_OUTER_BOUND('',#457,.T.);
#316=FACE_OUTER_BOUND('',#458,.T.);
#317=FACE_OUTER_BOUND('',#459,.T.);
#318=FACE_OUTER_BOUND('',#460,.T.);
#319=FACE_OUTER_BOUND('',#461,.T.);
#320=FACE_OUTER_BOUND('',#462,.T.);
#321=FACE_OUTER_BOUND('',#463,.T.);
#322=FACE_OUTER_BOUND('',#464,.T.);
#323=FACE_OUTER_BOUND('',#465,.T.);
#324=FACE_OUTER_BOUND('',#466,.T.);
#325=FACE_OUTER_BOUND('',#467,.T.);
#326=FACE_OUTER_BOUND('',#468,.T.);
#327=FACE_OUTER_BOUND('',#469,.T.);
#328=FACE_OUTER_BOUND('',#470,.T.);
#329=FACE_OUTER_BOUND('',#471,.T.);
#330=FACE_OUTER_BOUND('',#472,.T.);
#331=FACE_OUTER_BOUND('',#473,.T.);
#332=FACE_OUTER_BOUND('',#474,.T.);
#333=FACE_OUTER_BOUND('',#475,.T.);
#334=FACE_OUTER_BOUND('',#476,.T.);
#335=FACE_OUTER_BOUND('',#477,.T.);
#336=FACE_OUTER_BOUND('',#478,.T.);
#337=FACE_OUTER_BOUND('',#479,.T.);
#338=FACE_OUTER_BOUND('',#480,.T.);
#339=FACE_OUTER_BOUND('',#481,.T.);
#340=FACE_OUTER_BOUND('',#482,.T.);
#341=FACE_OUTER_BOUND('',#483,.T.);
#342=FACE_OUTER_BOUND('',#484,.T.);
#343=FACE_OUTER_BOUND('',#485,.T.);
#344=FACE_OUTER_BOUND('',#486,.T.);
#345=FACE_OUTER_BOUND('',#487,.T.);
#346=FACE_OUTER_BOUND('',#488,.T.);
#347=FACE_OUTER_BOUND('',#489,.T.);
#348=FACE_OUTER_BOUND('',#490,.T.);
#349=FACE_OUTER_BOUND('',#491,.T.);
#350=FACE_OUTER_BOUND('',#492,.T.);
#351=FACE_OUTER_BOUND('',#494,.T.);
#352=FACE_OUTER_BOUND('',#495,.T.);
#353=FACE_OUTER_BOUND('',#496,.T.);
#354=FACE_OUTER_BOUND('',#497,.T.);
#355=FACE_OUTER_BOUND('',#498,.T.);
#356=FACE_OUTER_BOUND('',#499,.T.);
#357=FACE_OUTER_BOUND('',#500,.T.);
#358=FACE_OUTER_BOUND('',#501,.T.);
#359=FACE_OUTER_BOUND('',#502,.T.);
#360=FACE_OUTER_BOUND('',#503,.T.);
#361=FACE_OUTER_BOUND('',#504,.T.);
#362=FACE_OUTER_BOUND('',#505,.T.);
#363=FACE_OUTER_BOUND('',#506,.T.);
#364=FACE_OUTER_BOUND('',#507,.T.);
#365=FACE_OUTER_BOUND('',#508,.T.);
#366=FACE_OUTER_BOUND('',#509,.T.);
#367=FACE_OUTER_BOUND('',#510,.T.);
#368=FACE_OUTER_BOUND('',#511,.T.);
#369=FACE_OUTER_BOUND('',#512,.T.);
#370=EDGE_LOOP('',(#1310,#1311,#1312,#1313));
#371=EDGE_LOOP('',(#1314,#1315,#1316,#1317));
#372=EDGE_LOOP('',(#1318));
#373=EDGE_LOOP('',(#1319));
#374=EDGE_LOOP('',(#1320));
#375=EDGE_LOOP('',(#1321));
#376=EDGE_LOOP('',(#1322,#1323,#1324,#1325,#1326));
#377=EDGE_LOOP('',(#1327,#1328,#1329,#1330,#1331));
#378=EDGE_LOOP('',(#1332,#1333,#1334,#1335,#1336,#1337));
#379=EDGE_LOOP('',(#1338,#1339,#1340,#1341));
#380=EDGE_LOOP('',(#1342,#1343,#1344,#1345));
#381=EDGE_LOOP('',(#1346));
#382=EDGE_LOOP('',(#1347));
#383=EDGE_LOOP('',(#1348,#1349,#1350,#1351));
#384=EDGE_LOOP('',(#1352,#1353));
#385=EDGE_LOOP('',(#1354,#1355));
#386=EDGE_LOOP('',(#1356,#1357,#1358,#1359));
#387=EDGE_LOOP('',(#1360,#1361));
#388=EDGE_LOOP('',(#1362,#1363));
#389=EDGE_LOOP('',(#1364,#1365,#1366,#1367,#1368));
#390=EDGE_LOOP('',(#1369,#1370,#1371,#1372));
#391=EDGE_LOOP('',(#1373,#1374,#1375,#1376));
#392=EDGE_LOOP('',(#1377,#1378,#1379,#1380));
#393=EDGE_LOOP('',(#1381,#1382,#1383,#1384));
#394=EDGE_LOOP('',(#1385,#1386,#1387,#1388));
#395=EDGE_LOOP('',(#1389,#1390,#1391,#1392));
#396=EDGE_LOOP('',(#1393,#1394,#1395,#1396));
#397=EDGE_LOOP('',(#1397,#1398,#1399,#1400));
#398=EDGE_LOOP('',(#1401,#1402,#1403,#1404));
#399=EDGE_LOOP('',(#1405,#1406,#1407,#1408,#1409,#1410));
#400=EDGE_LOOP('',(#1411,#1412,#1413,#1414,#1415));
#401=EDGE_LOOP('',(#1416,#1417,#1418,#1419));
#402=EDGE_LOOP('',(#1420,#1421,#1422,#1423));
#403=EDGE_LOOP('',(#1424));
#404=EDGE_LOOP('',(#1425));
#405=EDGE_LOOP('',(#1426));
#406=EDGE_LOOP('',(#1427));
#407=EDGE_LOOP('',(#1428));
#408=EDGE_LOOP('',(#1429));
#409=EDGE_LOOP('',(#1430));
#410=EDGE_LOOP('',(#1431));
#411=EDGE_LOOP('',(#1432));
#412=EDGE_LOOP('',(#1433));
#413=EDGE_LOOP('',(#1434));
#414=EDGE_LOOP('',(#1435));
#415=EDGE_LOOP('',(#1436,#1437,#1438,#1439));
#416=EDGE_LOOP('',(#1440,#1441,#1442,#1443));
#417=EDGE_LOOP('',(#1444));
#418=EDGE_LOOP('',(#1445));
#419=EDGE_LOOP('',(#1446));
#420=EDGE_LOOP('',(#1447));
#421=EDGE_LOOP('',(#1448,#1449,#1450,#1451));
#422=EDGE_LOOP('',(#1452,#1453,#1454,#1455));
#423=EDGE_LOOP('',(#1456,#1457,#1458,#1459));
#424=EDGE_LOOP('',(#1460,#1461,#1462,#1463));
#425=EDGE_LOOP('',(#1464,#1465,#1466,#1467));
#426=EDGE_LOOP('',(#1468));
#427=EDGE_LOOP('',(#1469));
#428=EDGE_LOOP('',(#1470));
#429=EDGE_LOOP('',(#1471,#1472,#1473,#1474));
#430=EDGE_LOOP('',(#1475));
#431=EDGE_LOOP('',(#1476,#1477,#1478,#1479,#1480,#1481,#1482,#1483));
#432=EDGE_LOOP('',(#1484,#1485,#1486,#1487));
#433=EDGE_LOOP('',(#1488,#1489,#1490,#1491,#1492,#1493,#1494,#1495));
#434=EDGE_LOOP('',(#1496,#1497,#1498,#1499));
#435=EDGE_LOOP('',(#1500));
#436=EDGE_LOOP('',(#1501));
#437=EDGE_LOOP('',(#1502));
#438=EDGE_LOOP('',(#1503,#1504,#1505,#1506));
#439=EDGE_LOOP('',(#1507,#1508,#1509,#1510));
#440=EDGE_LOOP('',(#1511,#1512,#1513,#1514));
#441=EDGE_LOOP('',(#1515));
#442=EDGE_LOOP('',(#1516,#1517,#1518,#1519));
#443=EDGE_LOOP('',(#1520,#1521,#1522,#1523));
#444=EDGE_LOOP('',(#1524,#1525,#1526,#1527));
#445=EDGE_LOOP('',(#1528,#1529,#1530,#1531));
#446=EDGE_LOOP('',(#1532));
#447=EDGE_LOOP('',(#1533));
#448=EDGE_LOOP('',(#1534,#1535,#1536,#1537));
#449=EDGE_LOOP('',(#1538));
#450=EDGE_LOOP('',(#1539));
#451=EDGE_LOOP('',(#1540,#1541,#1542,#1543));
#452=EDGE_LOOP('',(#1544,#1545,#1546,#1547));
#453=EDGE_LOOP('',(#1548,#1549,#1550,#1551));
#454=EDGE_LOOP('',(#1552,#1553,#1554,#1555));
#455=EDGE_LOOP('',(#1556,#1557,#1558,#1559));
#456=EDGE_LOOP('',(#1560,#1561,#1562,#1563));
#457=EDGE_LOOP('',(#1564,#1565,#1566,#1567));
#458=EDGE_LOOP('',(#1568,#1569,#1570,#1571));
#459=EDGE_LOOP('',(#1572,#1573,#1574,#1575));
#460=EDGE_LOOP('',(#1576,#1577,#1578,#1579));
#461=EDGE_LOOP('',(#1580,#1581,#1582,#1583));
#462=EDGE_LOOP('',(#1584,#1585,#1586,#1587));
#463=EDGE_LOOP('',(#1588,#1589,#1590,#1591));
#464=EDGE_LOOP('',(#1592,#1593,#1594,#1595));
#465=EDGE_LOOP('',(#1596,#1597,#1598,#1599));
#466=EDGE_LOOP('',(#1600,#1601,#1602,#1603));
#467=EDGE_LOOP('',(#1604,#1605,#1606,#1607));
#468=EDGE_LOOP('',(#1608,#1609,#1610,#1611,#1612,#1613,#1614,#1615,#1616));
#469=EDGE_LOOP('',(#1617,#1618,#1619,#1620));
#470=EDGE_LOOP('',(#1621,#1622,#1623,#1624));
#471=EDGE_LOOP('',(#1625,#1626,#1627,#1628));
#472=EDGE_LOOP('',(#1629,#1630,#1631,#1632));
#473=EDGE_LOOP('',(#1633,#1634,#1635,#1636));
#474=EDGE_LOOP('',(#1637,#1638,#1639,#1640));
#475=EDGE_LOOP('',(#1641,#1642,#1643,#1644));
#476=EDGE_LOOP('',(#1645,#1646,#1647,#1648));
#477=EDGE_LOOP('',(#1649,#1650,#1651,#1652));
#478=EDGE_LOOP('',(#1653,#1654,#1655,#1656));
#479=EDGE_LOOP('',(#1657,#1658,#1659,#1660));
#480=EDGE_LOOP('',(#1661,#1662,#1663,#1664));
#481=EDGE_LOOP('',(#1665,#1666,#1667,#1668,#1669,#1670,#1671,#1672,#1673,
#1674,#1675));
#482=EDGE_LOOP('',(#1676,#1677,#1678,#1679,#1680));
#483=EDGE_LOOP('',(#1681,#1682,#1683,#1684));
#484=EDGE_LOOP('',(#1685,#1686,#1687,#1688));
#485=EDGE_LOOP('',(#1689,#1690,#1691));
#486=EDGE_LOOP('',(#1692,#1693,#1694,#1695,#1696,#1697));
#487=EDGE_LOOP('',(#1698,#1699,#1700,#1701,#1702,#1703,#1704,#1705,#1706,
#1707,#1708,#1709,#1710,#1711,#1712,#1713,#1714,#1715,#1716,#1717,#1718,
#1719,#1720,#1721,#1722,#1723,#1724,#1725,#1726,#1727,#1728));
#488=EDGE_LOOP('',(#1729,#1730,#1731,#1732,#1733));
#489=EDGE_LOOP('',(#1734,#1735,#1736,#1737,#1738,#1739,#1740,#1741,#1742,
#1743,#1744,#1745,#1746,#1747,#1748,#1749,#1750,#1751,#1752,#1753,#1754,
#1755,#1756,#1757,#1758,#1759,#1760,#1761,#1762,#1763,#1764,#1765,#1766));
#490=EDGE_LOOP('',(#1767));
#491=EDGE_LOOP('',(#1768,#1769,#1770,#1771,#1772));
#492=EDGE_LOOP('',(#1773));
#493=EDGE_LOOP('',(#1774,#1775,#1776,#1777,#1778,#1779));
#494=EDGE_LOOP('',(#1780,#1781,#1782,#1783));
#495=EDGE_LOOP('',(#1784,#1785,#1786,#1787));
#496=EDGE_LOOP('',(#1788,#1789,#1790,#1791));
#497=EDGE_LOOP('',(#1792,#1793,#1794,#1795));
#498=EDGE_LOOP('',(#1796,#1797,#1798,#1799));
#499=EDGE_LOOP('',(#1800,#1801,#1802,#1803));
#500=EDGE_LOOP('',(#1804,#1805,#1806,#1807));
#501=EDGE_LOOP('',(#1808,#1809,#1810,#1811));
#502=EDGE_LOOP('',(#1812,#1813,#1814,#1815));
#503=EDGE_LOOP('',(#1816,#1817,#1818,#1819));
#504=EDGE_LOOP('',(#1820,#1821,#1822,#1823));
#505=EDGE_LOOP('',(#1824,#1825,#1826,#1827));
#506=EDGE_LOOP('',(#1828,#1829,#1830,#1831));
#507=EDGE_LOOP('',(#1832,#1833,#1834,#1835));
#508=EDGE_LOOP('',(#1836,#1837,#1838,#1839));
#509=EDGE_LOOP('',(#1840,#1841,#1842,#1843));
#510=EDGE_LOOP('',(#1844,#1845,#1846,#1847));
#511=EDGE_LOOP('',(#1848,#1849,#1850,#1851));
#512=EDGE_LOOP('',(#1852,#1853,#1854,#1855,#1856,#1857));
#513=LINE('',#2882,#649);
#514=LINE('',#2888,#650);
#515=LINE('',#2910,#651);
#516=LINE('',#2913,#652);
#517=LINE('',#2917,#653);
#518=LINE('',#2921,#654);
#519=LINE('',#2925,#655);
#520=LINE('',#2930,#656);
#521=LINE('',#2931,#657);
#522=LINE('',#2935,#658);
#523=LINE('',#2936,#659);
#524=LINE('',#2952,#660);
#525=LINE('',#2962,#661);
#526=LINE('',#2968,#662);
#527=LINE('',#2982,#663);
#528=LINE('',#2988,#664);
#529=LINE('',#2991,#665);
#530=LINE('',#2996,#666);
#531=LINE('',#3000,#667);
#532=LINE('',#3006,#668);
#533=LINE('',#3023,#669);
#534=LINE('',#3029,#670);
#535=LINE('',#3038,#671);
#536=LINE('',#3044,#672);
#537=LINE('',#3050,#673);
#538=LINE('',#3056,#674);
#539=LINE('',#3061,#675);
#540=LINE('',#3063,#676);
#541=LINE('',#3065,#677);
#542=LINE('',#3066,#678);
#543=LINE('',#3070,#679);
#544=LINE('',#3072,#680);
#545=LINE('',#3074,#681);
#546=LINE('',#3075,#682);
#547=LINE('',#3078,#683);
#548=LINE('',#3080,#684);
#549=LINE('',#3082,#685);
#550=LINE('',#3083,#686);
#551=LINE('',#3085,#687);
#552=LINE('',#3086,#688);
#553=LINE('',#3089,#689);
#554=LINE('',#3091,#690);
#555=LINE('',#3092,#691);
#556=LINE('',#3094,#692);
#557=LINE('',#3096,#693);
#558=LINE('',#3097,#694);
#559=LINE('',#3099,#695);
#560=LINE('',#3100,#696);
#561=LINE('',#3103,#697);
#562=LINE('',#3106,#698);
#563=LINE('',#3113,#699);
#564=LINE('',#3119,#700);
#565=LINE('',#3124,#701);
#566=LINE('',#3126,#702);
#567=LINE('',#3128,#703);
#568=LINE('',#3129,#704);
#569=LINE('',#3133,#705);
#570=LINE('',#3135,#706);
#571=LINE('',#3137,#707);
#572=LINE('',#3138,#708);
#573=LINE('',#3140,#709);
#574=LINE('',#3141,#710);
#575=LINE('',#3143,#711);
#576=LINE('',#3145,#712);
#577=LINE('',#3151,#713);
#578=LINE('',#3178,#714);
#579=LINE('',#3208,#715);
#580=LINE('',#3238,#716);
#581=LINE('',#3268,#717);
#582=LINE('',#3298,#718);
#583=LINE('',#3328,#719);
#584=LINE('',#3358,#720);
#585=LINE('',#3388,#721);
#586=LINE('',#3418,#722);
#587=LINE('',#3448,#723);
#588=LINE('',#3478,#724);
#589=LINE('',#3508,#725);
#590=LINE('',#3538,#726);
#591=LINE('',#3563,#727);
#592=LINE('',#3588,#728);
#593=LINE('',#3664,#729);
#594=LINE('',#3740,#730);
#595=LINE('',#3816,#731);
#596=LINE('',#3892,#732);
#597=LINE('',#3968,#733);
#598=LINE('',#4046,#734);
#599=LINE('',#4124,#735);
#600=LINE('',#4200,#736);
#601=LINE('',#4276,#737);
#602=LINE('',#4352,#738);
#603=LINE('',#4428,#739);
#604=LINE('',#4504,#740);
#605=LINE('',#4559,#741);
#606=LINE('',#4586,#742);
#607=LINE('',#9790,#743);
#608=LINE('',#9792,#744);
#609=LINE('',#9794,#745);
#610=LINE('',#9796,#746);
#611=LINE('',#9798,#747);
#612=LINE('',#9799,#748);
#613=LINE('',#9803,#749);
#614=LINE('',#9805,#750);
#615=LINE('',#9807,#751);
#616=LINE('',#9808,#752);
#617=LINE('',#9812,#753);
#618=LINE('',#9813,#754);
#619=LINE('',#9814,#755);
#620=LINE('',#9818,#756);
#621=LINE('',#9819,#757);
#622=LINE('',#9820,#758);
#623=LINE('',#9824,#759);
#624=LINE('',#9825,#760);
#625=LINE('',#9826,#761);
#626=LINE('',#9830,#762);
#627=LINE('',#9831,#763);
#628=LINE('',#9832,#764);
#629=LINE('',#9834,#765);
#630=LINE('',#9835,#766);
#631=LINE('',#9837,#767);
#632=LINE('',#9838,#768);
#633=LINE('',#9840,#769);
#634=LINE('',#9842,#770);
#635=LINE('',#9844,#771);
#636=LINE('',#9846,#772);
#637=LINE('',#9850,#773);
#638=LINE('',#9852,#774);
#639=LINE('',#9853,#775);
#640=LINE('',#9856,#776);
#641=LINE('',#9857,#777);
#642=LINE('',#9860,#778);
#643=LINE('',#9861,#779);
#644=LINE('',#9864,#780);
#645=LINE('',#9865,#781);
#646=LINE('',#9868,#782);
#647=LINE('',#9869,#783);
#648=LINE('',#9871,#784);
#649=VECTOR('',#2326,7.);
#650=VECTOR('',#2333,9.);
#651=VECTOR('',#2364,7.);
#652=VECTOR('',#2365,1000.);
#653=VECTOR('',#2368,1000.);
#654=VECTOR('',#2371,1000.);
#655=VECTOR('',#2374,1000.);
#656=VECTOR('',#2383,1000.);
#657=VECTOR('',#2384,1000.);
#658=VECTOR('',#2391,1000.);
#659=VECTOR('',#2392,1000.);
#660=VECTOR('',#2413,9.);
#661=VECTOR('',#2426,14.0000000000046);
#662=VECTOR('',#2433,13.9999999999978);
#663=VECTOR('',#2452,35.9999999999978);
#664=VECTOR('',#2459,48.0000000000047);
#665=VECTOR('',#2464,40.283264100914);
#666=VECTOR('',#2469,40.283264100914);
#667=VECTOR('',#2474,48.0000000000047);
#668=VECTOR('',#2481,36.0000000000017);
#669=VECTOR('',#2508,7.);
#670=VECTOR('',#2515,12.);
#671=VECTOR('',#2528,4.);
#672=VECTOR('',#2535,1.64999999999999);
#673=VECTOR('',#2542,1.64999999999999);
#674=VECTOR('',#2549,7.);
#675=VECTOR('',#2554,1000.);
#676=VECTOR('',#2555,1000.);
#677=VECTOR('',#2556,1000.);
#678=VECTOR('',#2557,1000.);
#679=VECTOR('',#2560,1000.);
#680=VECTOR('',#2561,1000.);
#681=VECTOR('',#2562,1000.);
#682=VECTOR('',#2563,1000.);
#683=VECTOR('',#2566,1000.);
#684=VECTOR('',#2567,1000.);
#685=VECTOR('',#2568,1000.);
#686=VECTOR('',#2569,1000.);
#687=VECTOR('',#2570,1000.);
#688=VECTOR('',#2571,1000.);
#689=VECTOR('',#2574,1000.);
#690=VECTOR('',#2575,1000.);
#691=VECTOR('',#2576,1000.);
#692=VECTOR('',#2579,1000.);
#693=VECTOR('',#2580,1000.);
#694=VECTOR('',#2581,1000.);
#695=VECTOR('',#2582,1000.);
#696=VECTOR('',#2583,1000.);
#697=VECTOR('',#2588,1000.);
#698=VECTOR('',#2593,1000.);
#699=VECTOR('',#2602,2.125);
#700=VECTOR('',#2609,2.25);
#701=VECTOR('',#2614,1000.);
#702=VECTOR('',#2615,1000.);
#703=VECTOR('',#2616,1000.);
#704=VECTOR('',#2617,1000.);
#705=VECTOR('',#2620,1000.);
#706=VECTOR('',#2621,1000.);
#707=VECTOR('',#2622,1000.);
#708=VECTOR('',#2623,1000.);
#709=VECTOR('',#2626,1000.);
#710=VECTOR('',#2627,1000.);
#711=VECTOR('',#2630,1000.);
#712=VECTOR('',#2633,1000.);
#713=VECTOR('',#2640,1.6211138875);
#714=VECTOR('',#2645,1.6211138875);
#715=VECTOR('',#2648,1.6211138875);
#716=VECTOR('',#2651,1.6211138875);
#717=VECTOR('',#2654,1.6211138875);
#718=VECTOR('',#2657,1.6211138875);
#719=VECTOR('',#2660,1.6211138875);
#720=VECTOR('',#2663,1.6211138875);
#721=VECTOR('',#2666,1.6211138875);
#722=VECTOR('',#2669,1.6211138875);
#723=VECTOR('',#2672,1.6211138875);
#724=VECTOR('',#2675,1.6211138875);
#725=VECTOR('',#2678,1.6211138875);
#726=VECTOR('',#2681,2.);
#727=VECTOR('',#2684,2.);
#728=VECTOR('',#2693,2.);
#729=VECTOR('',#2696,2.);
#730=VECTOR('',#2699,2.);
#731=VECTOR('',#2702,2.);
#732=VECTOR('',#2705,2.);
#733=VECTOR('',#2708,2.);
#734=VECTOR('',#2711,2.);
#735=VECTOR('',#2714,2.);
#736=VECTOR('',#2717,2.);
#737=VECTOR('',#2720,2.);
#738=VECTOR('',#2723,2.);
#739=VECTOR('',#2726,2.);
#740=VECTOR('',#2729,2.01);
#741=VECTOR('',#2734,2.01);
#742=VECTOR('',#2755,2.);
#743=VECTOR('',#2770,1000.);
#744=VECTOR('',#2771,1000.);
#745=VECTOR('',#2772,1000.);
#746=VECTOR('',#2773,1000.);
#747=VECTOR('',#2774,1000.);
#748=VECTOR('',#2775,1000.);
#749=VECTOR('',#2778,1000.);
#750=VECTOR('',#2779,1000.);
#751=VECTOR('',#2780,1000.);
#752=VECTOR('',#2781,1000.);
#753=VECTOR('',#2784,1000.);
#754=VECTOR('',#2785,1000.);
#755=VECTOR('',#2786,1000.);
#756=VECTOR('',#2789,1000.);
#757=VECTOR('',#2790,1000.);
#758=VECTOR('',#2791,1000.);
#759=VECTOR('',#2794,1000.);
#760=VECTOR('',#2795,1000.);
#761=VECTOR('',#2796,1000.);
#762=VECTOR('',#2799,1000.);
#763=VECTOR('',#2800,1000.);
#764=VECTOR('',#2801,1000.);
#765=VECTOR('',#2804,1000.);
#766=VECTOR('',#2805,1000.);
#767=VECTOR('',#2808,1000.);
#768=VECTOR('',#2809,1000.);
#769=VECTOR('',#2812,1000.);
#770=VECTOR('',#2815,1000.);
#771=VECTOR('',#2818,1000.);
#772=VECTOR('',#2821,1000.);
#773=VECTOR('',#2826,1000.);
#774=VECTOR('',#2827,1000.);
#775=VECTOR('',#2828,1000.);
#776=VECTOR('',#2831,1000.);
#777=VECTOR('',#2832,1000.);
#778=VECTOR('',#2835,1000.);
#779=VECTOR('',#2836,1000.);
#780=VECTOR('',#2839,1000.);
#781=VECTOR('',#2840,1000.);
#782=VECTOR('',#2843,1000.);
#783=VECTOR('',#2844,1000.);
#784=VECTOR('',#2847,1000.);
#785=CIRCLE('',#2110,7.);
#786=CIRCLE('',#2111,7.);
#787=CIRCLE('',#2113,9.);
#788=CIRCLE('',#2114,9.);
#789=CIRCLE('',#2119,6.);
#790=CIRCLE('',#2120,1.);
#791=CIRCLE('',#2121,7.);
#792=CIRCLE('',#2122,7.);
#793=CIRCLE('',#2124,7.);
#794=CIRCLE('',#2125,7.);
#795=CIRCLE('',#2126,1.);
#796=CIRCLE('',#2127,6.);
#797=CIRCLE('',#2129,7.);
#798=CIRCLE('',#2130,7.);
#799=CIRCLE('',#2131,7.);
#800=CIRCLE('',#2132,7.);
#801=CIRCLE('',#2143,40.283264100914);
#802=CIRCLE('',#2144,2.);
#803=CIRCLE('',#2145,40.283264100914);
#804=CIRCLE('',#2146,40.283264100914);
#805=CIRCLE('',#2148,9.);
#806=CIRCLE('',#2149,9.);
#807=CIRCLE('',#2151,16.0000000000017);
#808=CIRCLE('',#2152,2.);
#809=CIRCLE('',#2153,14.0000000000046);
#810=CIRCLE('',#2155,14.0000000000046);
#811=CIRCLE('',#2157,13.9999999999978);
#812=CIRCLE('',#2158,13.9999999999978);
#813=CIRCLE('',#2160,2.);
#814=CIRCLE('',#2161,15.9999999999978);
#815=CIRCLE('',#2163,33.9999999999978);
#816=CIRCLE('',#2164,2.);
#817=CIRCLE('',#2165,35.9999999999978);
#818=CIRCLE('',#2167,35.9999999999978);
#819=CIRCLE('',#2169,48.0000000000047);
#820=CIRCLE('',#2170,48.0000000000047);
#821=CIRCLE('',#2173,48.0000000000047);
#822=CIRCLE('',#2174,48.0000000000047);
#823=CIRCLE('',#2176,48.0000000000047);
#824=CIRCLE('',#2178,36.0000000000017);
#825=CIRCLE('',#2179,36.0000000000017);
#826=CIRCLE('',#2181,2.);
#827=CIRCLE('',#2182,34.0000000000017);
#828=CIRCLE('',#2191,7.);
#829=CIRCLE('',#2192,7.);
#830=CIRCLE('',#2194,12.);
#831=CIRCLE('',#2195,12.);
#832=CIRCLE('',#2200,4.);
#833=CIRCLE('',#2201,4.);
#834=CIRCLE('',#2203,1.64999999999999);
#835=CIRCLE('',#2204,1.64999999999999);
#836=CIRCLE('',#2206,1.64999999999999);
#837=CIRCLE('',#2207,1.64999999999999);
#838=CIRCLE('',#2209,7.);
#839=CIRCLE('',#2210,7.);
#840=CIRCLE('',#2223,2.125);
#841=CIRCLE('',#2224,2.125);
#842=CIRCLE('',#2226,2.25);
#843=CIRCLE('',#2227,2.25);
#844=CIRCLE('',#2236,1.6211138875);
#845=CIRCLE('',#2250,2.);
#846=CIRCLE('',#2251,2.);
#847=CIRCLE('',#2252,2.);
#848=CIRCLE('',#2253,2.);
#849=CIRCLE('',#2267,2.);
#850=CIRCLE('',#2268,1.6211138875);
#851=CIRCLE('',#2269,1.55999999999999);
#852=CIRCLE('',#2270,1.6211138875);
#853=CIRCLE('',#2272,2.11715728752538);
#854=CIRCLE('',#2273,0.4);
#855=CIRCLE('',#2275,3.9385786437627);
#856=CIRCLE('',#2276,0.1);
#857=CIRCLE('',#2277,4.00928932188135);
#858=CIRCLE('',#2280,2.);
#859=VERTEX_POINT('',#2879);
#860=VERTEX_POINT('',#2881);
#861=VERTEX_POINT('',#2885);
#862=VERTEX_POINT('',#2887);
#863=VERTEX_POINT('',#2894);
#864=VERTEX_POINT('',#2896);
#865=VERTEX_POINT('',#2898);
#866=VERTEX_POINT('',#2902);
#867=VERTEX_POINT('',#2903);
#868=VERTEX_POINT('',#2906);
#869=VERTEX_POINT('',#2911);
#870=VERTEX_POINT('',#2912);
#871=VERTEX_POINT('',#2914);
#872=VERTEX_POINT('',#2916);
#873=VERTEX_POINT('',#2919);
#874=VERTEX_POINT('',#2920);
#875=VERTEX_POINT('',#2922);
#876=VERTEX_POINT('',#2924);
#877=VERTEX_POINT('',#2941);
#878=VERTEX_POINT('',#2943);
#879=VERTEX_POINT('',#2945);
#880=VERTEX_POINT('',#2949);
#881=VERTEX_POINT('',#2951);
#882=VERTEX_POINT('',#2955);
#883=VERTEX_POINT('',#2957);
#884=VERTEX_POINT('',#2961);
#885=VERTEX_POINT('',#2965);
#886=VERTEX_POINT('',#2967);
#887=VERTEX_POINT('',#2971);
#888=VERTEX_POINT('',#2975);
#889=VERTEX_POINT('',#2977);
#890=VERTEX_POINT('',#2981);
#891=VERTEX_POINT('',#2985);
#892=VERTEX_POINT('',#2987);
#893=VERTEX_POINT('',#2993);
#894=VERTEX_POINT('',#2994);
#895=VERTEX_POINT('',#2999);
#896=VERTEX_POINT('',#3003);
#897=VERTEX_POINT('',#3005);
#898=VERTEX_POINT('',#3009);
#899=VERTEX_POINT('',#3020);
#900=VERTEX_POINT('',#3022);
#901=VERTEX_POINT('',#3026);
#902=VERTEX_POINT('',#3028);
#903=VERTEX_POINT('',#3035);
#904=VERTEX_POINT('',#3037);
#905=VERTEX_POINT('',#3041);
#906=VERTEX_POINT('',#3043);
#907=VERTEX_POINT('',#3047);
#908=VERTEX_POINT('',#3049);
#909=VERTEX_POINT('',#3053);
#910=VERTEX_POINT('',#3055);
#911=VERTEX_POINT('',#3059);
#912=VERTEX_POINT('',#3060);
#913=VERTEX_POINT('',#3062);
#914=VERTEX_POINT('',#3064);
#915=VERTEX_POINT('',#3068);
#916=VERTEX_POINT('',#3069);
#917=VERTEX_POINT('',#3071);
#918=VERTEX_POINT('',#3073);
#919=VERTEX_POINT('',#3077);
#920=VERTEX_POINT('',#3079);
#921=VERTEX_POINT('',#3081);
#922=VERTEX_POINT('',#3084);
#923=VERTEX_POINT('',#3088);
#924=VERTEX_POINT('',#3090);
#925=VERTEX_POINT('',#3095);
#926=VERTEX_POINT('',#3098);
#927=VERTEX_POINT('',#3110);
#928=VERTEX_POINT('',#3112);
#929=VERTEX_POINT('',#3116);
#930=VERTEX_POINT('',#3118);
#931=VERTEX_POINT('',#3122);
#932=VERTEX_POINT('',#3123);
#933=VERTEX_POINT('',#3125);
#934=VERTEX_POINT('',#3127);
#935=VERTEX_POINT('',#3131);
#936=VERTEX_POINT('',#3132);
#937=VERTEX_POINT('',#3134);
#938=VERTEX_POINT('',#3136);
#939=VERTEX_POINT('',#3149);
#940=VERTEX_POINT('',#3150);
#941=VERTEX_POINT('',#3152);
#942=VERTEX_POINT('',#3164);
#943=VERTEX_POINT('',#3176);
#944=VERTEX_POINT('',#3177);
#945=VERTEX_POINT('',#3206);
#946=VERTEX_POINT('',#3207);
#947=VERTEX_POINT('',#3236);
#948=VERTEX_POINT('',#3237);
#949=VERTEX_POINT('',#3266);
#950=VERTEX_POINT('',#3267);
#951=VERTEX_POINT('',#3296);
#952=VERTEX_POINT('',#3297);
#953=VERTEX_POINT('',#3326);
#954=VERTEX_POINT('',#3327);
#955=VERTEX_POINT('',#3356);
#956=VERTEX_POINT('',#3357);
#957=VERTEX_POINT('',#3386);
#958=VERTEX_POINT('',#3387);
#959=VERTEX_POINT('',#3416);
#960=VERTEX_POINT('',#3417);
#961=VERTEX_POINT('',#3446);
#962=VERTEX_POINT('',#3447);
#963=VERTEX_POINT('',#3476);
#964=VERTEX_POINT('',#3477);
#965=VERTEX_POINT('',#3506);
#966=VERTEX_POINT('',#3507);
#967=VERTEX_POINT('',#3536);
#968=VERTEX_POINT('',#3537);
#969=VERTEX_POINT('',#3539);
#970=VERTEX_POINT('',#3560);
#971=VERTEX_POINT('',#3562);
#972=VERTEX_POINT('',#3564);
#973=VERTEX_POINT('',#3567);
#974=VERTEX_POINT('',#3586);
#975=VERTEX_POINT('',#3587);
#976=VERTEX_POINT('',#3662);
#977=VERTEX_POINT('',#3663);
#978=VERTEX_POINT('',#3738);
#979=VERTEX_POINT('',#3739);
#980=VERTEX_POINT('',#3814);
#981=VERTEX_POINT('',#3815);
#982=VERTEX_POINT('',#3890);
#983=VERTEX_POINT('',#3891);
#984=VERTEX_POINT('',#3966);
#985=VERTEX_POINT('',#3967);
#986=VERTEX_POINT('',#4044);
#987=VERTEX_POINT('',#4045);
#988=VERTEX_POINT('',#4122);
#989=VERTEX_POINT('',#4123);
#990=VERTEX_POINT('',#4198);
#991=VERTEX_POINT('',#4199);
#992=VERTEX_POINT('',#4274);
#993=VERTEX_POINT('',#4275);
#994=VERTEX_POINT('',#4350);
#995=VERTEX_POINT('',#4351);
#996=VERTEX_POINT('',#4426);
#997=VERTEX_POINT('',#4427);
#998=VERTEX_POINT('',#4502);
#999=VERTEX_POINT('',#4503);
#1000=VERTEX_POINT('',#4505);
#1001=VERTEX_POINT('',#4507);
#1002=VERTEX_POINT('',#4518);
#1003=VERTEX_POINT('',#4537);
#1004=VERTEX_POINT('',#4556);
#1005=VERTEX_POINT('',#4558);
#1006=VERTEX_POINT('',#4561);
#1007=VERTEX_POINT('',#4576);
#1008=VERTEX_POINT('',#4580);
#1009=VERTEX_POINT('',#4582);
#1010=VERTEX_POINT('',#4588);
#1011=VERTEX_POINT('',#4595);
#1012=VERTEX_POINT('',#9788);
#1013=VERTEX_POINT('',#9789);
#1014=VERTEX_POINT('',#9791);
#1015=VERTEX_POINT('',#9793);
#1016=VERTEX_POINT('',#9795);
#1017=VERTEX_POINT('',#9797);
#1018=VERTEX_POINT('',#9801);
#1019=VERTEX_POINT('',#9802);
#1020=VERTEX_POINT('',#9804);
#1021=VERTEX_POINT('',#9806);
#1022=VERTEX_POINT('',#9810);
#1023=VERTEX_POINT('',#9811);
#1024=VERTEX_POINT('',#9816);
#1025=VERTEX_POINT('',#9817);
#1026=VERTEX_POINT('',#9822);
#1027=VERTEX_POINT('',#9823);
#1028=VERTEX_POINT('',#9828);
#1029=VERTEX_POINT('',#9829);
#1030=VERTEX_POINT('',#9849);
#1031=VERTEX_POINT('',#9851);
#1032=VERTEX_POINT('',#9855);
#1033=VERTEX_POINT('',#9859);
#1034=VERTEX_POINT('',#9863);
#1035=VERTEX_POINT('',#9867);
#1036=EDGE_CURVE('',#859,#859,#785,.T.);
#1037=EDGE_CURVE('',#859,#860,#513,.T.);
#1038=EDGE_CURVE('',#860,#860,#786,.T.);
#1039=EDGE_CURVE('',#861,#861,#787,.T.);
#1040=EDGE_CURVE('',#861,#862,#514,.T.);
#1041=EDGE_CURVE('',#862,#862,#788,.T.);
#1042=EDGE_CURVE('',#863,#863,#789,.T.);
#1043=EDGE_CURVE('',#863,#864,#790,.T.);
#1044=EDGE_CURVE('',#865,#864,#791,.T.);
#1045=EDGE_CURVE('',#864,#865,#792,.T.);
#1046=EDGE_CURVE('',#866,#867,#793,.T.);
#1047=EDGE_CURVE('',#867,#866,#794,.T.);
#1048=EDGE_CURVE('',#867,#868,#795,.T.);
#1049=EDGE_CURVE('',#868,#868,#796,.T.);
#1050=EDGE_CURVE('',#866,#865,#515,.T.);
#1051=EDGE_CURVE('',#869,#870,#516,.T.);
#1052=EDGE_CURVE('',#869,#871,#797,.T.);
#1053=EDGE_CURVE('',#872,#871,#517,.T.);
#1054=EDGE_CURVE('',#870,#872,#798,.T.);
#1055=EDGE_CURVE('',#873,#874,#518,.T.);
#1056=EDGE_CURVE('',#873,#875,#799,.T.);
#1057=EDGE_CURVE('',#876,#875,#519,.T.);
#1058=EDGE_CURVE('',#874,#876,#800,.T.);
#1059=EDGE_CURVE('',#876,#874,#520,.T.);
#1060=EDGE_CURVE('',#875,#873,#521,.T.);
#1061=EDGE_CURVE('',#871,#869,#522,.T.);
#1062=EDGE_CURVE('',#872,#870,#523,.T.);
#1063=EDGE_CURVE('',#877,#877,#801,.T.);
#1064=EDGE_CURVE('',#877,#878,#802,.T.);
#1065=EDGE_CURVE('',#878,#879,#803,.T.);
#1066=EDGE_CURVE('',#879,#878,#804,.T.);
#1067=EDGE_CURVE('',#880,#880,#805,.T.);
#1068=EDGE_CURVE('',#880,#881,#524,.T.);
#1069=EDGE_CURVE('',#881,#881,#806,.T.);
#1070=EDGE_CURVE('',#882,#882,#807,.T.);
#1071=EDGE_CURVE('',#882,#883,#808,.T.);
#1072=EDGE_CURVE('',#883,#883,#809,.T.);
#1073=EDGE_CURVE('',#883,#884,#525,.T.);
#1074=EDGE_CURVE('',#884,#884,#810,.T.);
#1075=EDGE_CURVE('',#885,#885,#811,.T.);
#1076=EDGE_CURVE('',#885,#886,#526,.T.);
#1077=EDGE_CURVE('',#886,#886,#812,.T.);
#1078=EDGE_CURVE('',#886,#887,#813,.T.);
#1079=EDGE_CURVE('',#887,#887,#814,.T.);
#1080=EDGE_CURVE('',#888,#888,#815,.T.);
#1081=EDGE_CURVE('',#888,#889,#816,.T.);
#1082=EDGE_CURVE('',#889,#889,#817,.T.);
#1083=EDGE_CURVE('',#889,#890,#527,.T.);
#1084=EDGE_CURVE('',#890,#890,#818,.T.);
#1085=EDGE_CURVE('',#891,#891,#819,.T.);
#1086=EDGE_CURVE('',#891,#892,#528,.T.);
#1087=EDGE_CURVE('',#892,#892,#820,.T.);
#1088=EDGE_CURVE('',#892,#877,#529,.T.);
#1089=EDGE_CURVE('',#893,#894,#821,.T.);
#1090=EDGE_CURVE('',#894,#879,#530,.T.);
#1091=EDGE_CURVE('',#894,#893,#822,.T.);
#1092=EDGE_CURVE('',#893,#895,#531,.T.);
#1093=EDGE_CURVE('',#895,#895,#823,.T.);
#1094=EDGE_CURVE('',#896,#896,#824,.T.);
#1095=EDGE_CURVE('',#896,#897,#532,.T.);
#1096=EDGE_CURVE('',#897,#897,#825,.T.);
#1097=EDGE_CURVE('',#897,#898,#826,.T.);
#1098=EDGE_CURVE('',#898,#898,#827,.T.);
#1099=EDGE_CURVE('',#899,#899,#828,.T.);
#1100=EDGE_CURVE('',#899,#900,#533,.T.);
#1101=EDGE_CURVE('',#900,#900,#829,.T.);
#1102=EDGE_CURVE('',#901,#901,#830,.T.);
#1103=EDGE_CURVE('',#901,#902,#534,.T.);
#1104=EDGE_CURVE('',#902,#902,#831,.T.);
#1105=EDGE_CURVE('',#903,#903,#832,.T.);
#1106=EDGE_CURVE('',#903,#904,#535,.T.);
#1107=EDGE_CURVE('',#904,#904,#833,.T.);
#1108=EDGE_CURVE('',#905,#905,#834,.T.);
#1109=EDGE_CURVE('',#905,#906,#536,.T.);
#1110=EDGE_CURVE('',#906,#906,#835,.T.);
#1111=EDGE_CURVE('',#907,#907,#836,.T.);
#1112=EDGE_CURVE('',#907,#908,#537,.T.);
#1113=EDGE_CURVE('',#908,#908,#837,.T.);
#1114=EDGE_CURVE('',#909,#909,#838,.T.);
#1115=EDGE_CURVE('',#909,#910,#538,.T.);
#1116=EDGE_CURVE('',#910,#910,#839,.T.);
#1117=EDGE_CURVE('',#911,#912,#539,.T.);
#1118=EDGE_CURVE('',#913,#912,#540,.T.);
#1119=EDGE_CURVE('',#913,#914,#541,.T.);
#1120=EDGE_CURVE('',#911,#914,#542,.T.);
#1121=EDGE_CURVE('',#915,#916,#543,.T.);
#1122=EDGE_CURVE('',#917,#916,#544,.T.);
#1123=EDGE_CURVE('',#918,#917,#545,.T.);
#1124=EDGE_CURVE('',#918,#915,#546,.T.);
#1125=EDGE_CURVE('',#916,#919,#547,.T.);
#1126=EDGE_CURVE('',#920,#919,#548,.T.);
#1127=EDGE_CURVE('',#921,#920,#549,.T.);
#1128=EDGE_CURVE('',#921,#914,#550,.T.);
#1129=EDGE_CURVE('',#922,#913,#551,.T.);
#1130=EDGE_CURVE('',#917,#922,#552,.T.);
#1131=EDGE_CURVE('',#919,#923,#553,.T.);
#1132=EDGE_CURVE('',#924,#923,#554,.T.);
#1133=EDGE_CURVE('',#920,#924,#555,.T.);
#1134=EDGE_CURVE('',#923,#915,#556,.T.);
#1135=EDGE_CURVE('',#925,#918,#557,.T.);
#1136=EDGE_CURVE('',#925,#912,#558,.T.);
#1137=EDGE_CURVE('',#926,#911,#559,.T.);
#1138=EDGE_CURVE('',#924,#926,#560,.T.);
#1139=EDGE_CURVE('',#926,#921,#561,.T.);
#1140=EDGE_CURVE('',#922,#925,#562,.T.);
#1141=EDGE_CURVE('',#927,#927,#840,.T.);
#1142=EDGE_CURVE('',#927,#928,#563,.T.);
#1143=EDGE_CURVE('',#928,#928,#841,.T.);
#1144=EDGE_CURVE('',#929,#929,#842,.T.);
#1145=EDGE_CURVE('',#929,#930,#564,.T.);
#1146=EDGE_CURVE('',#930,#930,#843,.T.);
#1147=EDGE_CURVE('',#931,#932,#565,.T.);
#1148=EDGE_CURVE('',#932,#933,#566,.T.);
#1149=EDGE_CURVE('',#933,#934,#567,.T.);
#1150=EDGE_CURVE('',#934,#931,#568,.T.);
#1151=EDGE_CURVE('',#935,#936,#569,.T.);
#1152=EDGE_CURVE('',#937,#935,#570,.T.);
#1153=EDGE_CURVE('',#938,#937,#571,.T.);
#1154=EDGE_CURVE('',#936,#938,#572,.T.);
#1155=EDGE_CURVE('',#932,#936,#573,.T.);
#1156=EDGE_CURVE('',#931,#935,#574,.T.);
#1157=EDGE_CURVE('',#933,#938,#575,.T.);
#1158=EDGE_CURVE('',#934,#937,#576,.T.);
#1159=EDGE_CURVE('',#939,#940,#577,.T.);
#1160=EDGE_CURVE('',#941,#939,#101,.T.);
#1161=EDGE_CURVE('',#941,#942,#844,.T.);
#1162=EDGE_CURVE('',#942,#940,#102,.T.);
#1163=EDGE_CURVE('',#943,#944,#578,.T.);
#1164=EDGE_CURVE('',#939,#943,#103,.T.);
#1165=EDGE_CURVE('',#940,#944,#104,.T.);
#1166=EDGE_CURVE('',#945,#946,#579,.T.);
#1167=EDGE_CURVE('',#943,#945,#105,.T.);
#1168=EDGE_CURVE('',#944,#946,#106,.T.);
#1169=EDGE_CURVE('',#947,#948,#580,.T.);
#1170=EDGE_CURVE('',#945,#947,#107,.T.);
#1171=EDGE_CURVE('',#946,#948,#108,.T.);
#1172=EDGE_CURVE('',#949,#950,#581,.T.);
#1173=EDGE_CURVE('',#947,#949,#109,.T.);
#1174=EDGE_CURVE('',#948,#950,#110,.T.);
#1175=EDGE_CURVE('',#951,#952,#582,.T.);
#1176=EDGE_CURVE('',#949,#951,#111,.T.);
#1177=EDGE_CURVE('',#950,#952,#112,.T.);
#1178=EDGE_CURVE('',#953,#954,#583,.T.);
#1179=EDGE_CURVE('',#951,#953,#113,.T.);
#1180=EDGE_CURVE('',#952,#954,#114,.T.);
#1181=EDGE_CURVE('',#955,#956,#584,.T.);
#1182=EDGE_CURVE('',#953,#955,#115,.T.);
#1183=EDGE_CURVE('',#954,#956,#116,.T.);
#1184=EDGE_CURVE('',#957,#958,#585,.T.);
#1185=EDGE_CURVE('',#955,#957,#117,.T.);
#1186=EDGE_CURVE('',#956,#958,#118,.T.);
#1187=EDGE_CURVE('',#959,#960,#586,.T.);
#1188=EDGE_CURVE('',#957,#959,#119,.T.);
#1189=EDGE_CURVE('',#958,#960,#120,.T.);
#1190=EDGE_CURVE('',#961,#962,#587,.T.);
#1191=EDGE_CURVE('',#959,#961,#121,.T.);
#1192=EDGE_CURVE('',#960,#962,#122,.T.);
#1193=EDGE_CURVE('',#963,#964,#588,.T.);
#1194=EDGE_CURVE('',#961,#963,#123,.T.);
#1195=EDGE_CURVE('',#962,#964,#124,.T.);
#1196=EDGE_CURVE('',#965,#966,#589,.T.);
#1197=EDGE_CURVE('',#963,#965,#125,.T.);
#1198=EDGE_CURVE('',#964,#966,#126,.T.);
#1199=EDGE_CURVE('',#967,#968,#590,.T.);
#1200=EDGE_CURVE('',#969,#967,#65,.F.);
#1201=EDGE_CURVE('',#969,#970,#845,.T.);
#1202=EDGE_CURVE('',#970,#971,#591,.T.);
#1203=EDGE_CURVE('',#971,#972,#846,.T.);
#1204=EDGE_CURVE('',#972,#971,#847,.T.);
#1205=EDGE_CURVE('',#970,#973,#848,.T.);
#1206=EDGE_CURVE('',#973,#968,#66,.T.);
#1207=EDGE_CURVE('',#974,#975,#592,.T.);
#1208=EDGE_CURVE('',#967,#974,#67,.F.);
#1209=EDGE_CURVE('',#968,#975,#68,.T.);
#1210=EDGE_CURVE('',#976,#977,#593,.T.);
#1211=EDGE_CURVE('',#974,#976,#69,.F.);
#1212=EDGE_CURVE('',#975,#977,#70,.T.);
#1213=EDGE_CURVE('',#978,#979,#594,.T.);
#1214=EDGE_CURVE('',#976,#978,#71,.F.);
#1215=EDGE_CURVE('',#977,#979,#72,.T.);
#1216=EDGE_CURVE('',#980,#981,#595,.T.);
#1217=EDGE_CURVE('',#978,#980,#73,.F.);
#1218=EDGE_CURVE('',#979,#981,#74,.T.);
#1219=EDGE_CURVE('',#982,#983,#596,.T.);
#1220=EDGE_CURVE('',#980,#982,#75,.F.);
#1221=EDGE_CURVE('',#981,#983,#76,.T.);
#1222=EDGE_CURVE('',#984,#985,#597,.T.);
#1223=EDGE_CURVE('',#982,#984,#77,.F.);
#1224=EDGE_CURVE('',#983,#985,#78,.T.);
#1225=EDGE_CURVE('',#986,#987,#598,.T.);
#1226=EDGE_CURVE('',#984,#986,#79,.F.);
#1227=EDGE_CURVE('',#985,#987,#80,.T.);
#1228=EDGE_CURVE('',#988,#989,#599,.T.);
#1229=EDGE_CURVE('',#986,#988,#81,.F.);
#1230=EDGE_CURVE('',#987,#989,#82,.T.);
#1231=EDGE_CURVE('',#990,#991,#600,.T.);
#1232=EDGE_CURVE('',#988,#990,#83,.F.);
#1233=EDGE_CURVE('',#989,#991,#84,.T.);
#1234=EDGE_CURVE('',#992,#993,#601,.T.);
#1235=EDGE_CURVE('',#990,#992,#85,.F.);
#1236=EDGE_CURVE('',#991,#993,#86,.T.);
#1237=EDGE_CURVE('',#994,#995,#602,.T.);
#1238=EDGE_CURVE('',#992,#994,#87,.F.);
#1239=EDGE_CURVE('',#993,#995,#88,.T.);
#1240=EDGE_CURVE('',#996,#997,#603,.T.);
#1241=EDGE_CURVE('',#994,#996,#89,.F.);
#1242=EDGE_CURVE('',#995,#997,#90,.T.);
#1243=EDGE_CURVE('',#998,#999,#604,.T.);
#1244=EDGE_CURVE('',#1000,#998,#849,.T.);
#1245=EDGE_CURVE('',#1000,#1001,#91,.T.);
#1246=EDGE_CURVE('',#1001,#1002,#92,.T.);
#1247=EDGE_CURVE('',#1002,#1003,#93,.T.);
#1248=EDGE_CURVE('',#1003,#1004,#850,.T.);
#1249=EDGE_CURVE('',#1004,#1005,#605,.T.);
#1250=EDGE_CURVE('',#1005,#1005,#851,.T.);
#1251=EDGE_CURVE('',#1004,#1006,#852,.T.);
#1252=EDGE_CURVE('',#1006,#999,#94,.T.);
#1253=EDGE_CURVE('',#1007,#1007,#853,.T.);
#1254=EDGE_CURVE('',#1007,#972,#854,.T.);
#1255=EDGE_CURVE('',#1008,#1008,#855,.T.);
#1256=EDGE_CURVE('',#1008,#1009,#856,.T.);
#1257=EDGE_CURVE('',#1009,#1009,#857,.T.);
#1258=EDGE_CURVE('',#1009,#1007,#606,.T.);
#1259=EDGE_CURVE('',#999,#1010,#95,.T.);
#1260=EDGE_CURVE('',#998,#1010,#858,.T.);
#1261=EDGE_CURVE('',#997,#1011,#96,.T.);
#1262=EDGE_CURVE('',#1011,#1000,#97,.T.);
#1263=EDGE_CURVE('',#996,#1010,#98,.F.);
#1264=EDGE_CURVE('',#942,#969,#99,.T.);
#1265=EDGE_CURVE('',#966,#1006,#127,.T.);
#1266=EDGE_CURVE('',#965,#1003,#128,.T.);
#1267=EDGE_CURVE('',#973,#941,#100,.T.);
#1268=EDGE_CURVE('',#1012,#1013,#607,.T.);
#1269=EDGE_CURVE('',#1013,#1014,#608,.T.);
#1270=EDGE_CURVE('',#1014,#1015,#609,.T.);
#1271=EDGE_CURVE('',#1015,#1016,#610,.T.);
#1272=EDGE_CURVE('',#1016,#1017,#611,.T.);
#1273=EDGE_CURVE('',#1017,#1012,#612,.T.);
#1274=EDGE_CURVE('',#1018,#1019,#613,.T.);
#1275=EDGE_CURVE('',#1019,#1020,#614,.T.);
#1276=EDGE_CURVE('',#1021,#1020,#615,.T.);
#1277=EDGE_CURVE('',#1018,#1021,#616,.T.);
#1278=EDGE_CURVE('',#1022,#1023,#617,.T.);
#1279=EDGE_CURVE('',#1023,#1019,#618,.T.);
#1280=EDGE_CURVE('',#1022,#1018,#619,.T.);
#1281=EDGE_CURVE('',#1024,#1025,#620,.T.);
#1282=EDGE_CURVE('',#1025,#1023,#621,.T.);
#1283=EDGE_CURVE('',#1024,#1022,#622,.T.);
#1284=EDGE_CURVE('',#1026,#1027,#623,.T.);
#1285=EDGE_CURVE('',#1027,#1025,#624,.T.);
#1286=EDGE_CURVE('',#1026,#1024,#625,.T.);
#1287=EDGE_CURVE('',#1028,#1029,#626,.T.);
#1288=EDGE_CURVE('',#1029,#1027,#627,.T.);
#1289=EDGE_CURVE('',#1028,#1026,#628,.T.);
#1290=EDGE_CURVE('',#1020,#1029,#629,.T.);
#1291=EDGE_CURVE('',#1021,#1028,#630,.T.);
#1292=EDGE_CURVE('',#1017,#1023,#631,.T.);
#1293=EDGE_CURVE('',#1019,#1016,#632,.T.);
#1294=EDGE_CURVE('',#1020,#1015,#633,.T.);
#1295=EDGE_CURVE('',#1012,#1025,#634,.T.);
#1296=EDGE_CURVE('',#1029,#1014,#635,.T.);
#1297=EDGE_CURVE('',#1013,#1027,#636,.T.);
#1298=EDGE_CURVE('',#1030,#1021,#637,.T.);
#1299=EDGE_CURVE('',#1031,#1030,#638,.T.);
#1300=EDGE_CURVE('',#1031,#1018,#639,.T.);
#1301=EDGE_CURVE('',#1032,#1031,#640,.T.);
#1302=EDGE_CURVE('',#1032,#1022,#641,.T.);
#1303=EDGE_CURVE('',#1033,#1032,#642,.T.);
#1304=EDGE_CURVE('',#1033,#1024,#643,.T.);
#1305=EDGE_CURVE('',#1034,#1033,#644,.T.);
#1306=EDGE_CURVE('',#1034,#1026,#645,.T.);
#1307=EDGE_CURVE('',#1035,#1034,#646,.T.);
#1308=EDGE_CURVE('',#1035,#1028,#647,.T.);
#1309=EDGE_CURVE('',#1030,#1035,#648,.T.);
#1310=ORIENTED_EDGE('',*,*,#1036,.T.);
#1311=ORIENTED_EDGE('',*,*,#1037,.T.);
#1312=ORIENTED_EDGE('',*,*,#1038,.F.);
#1313=ORIENTED_EDGE('',*,*,#1037,.F.);
#1314=ORIENTED_EDGE('',*,*,#1039,.T.);
#1315=ORIENTED_EDGE('',*,*,#1040,.T.);
#1316=ORIENTED_EDGE('',*,*,#1041,.F.);
#1317=ORIENTED_EDGE('',*,*,#1040,.F.);
#1318=ORIENTED_EDGE('',*,*,#1041,.T.);
#1319=ORIENTED_EDGE('',*,*,#1036,.F.);
#1320=ORIENTED_EDGE('',*,*,#1039,.F.);
#1321=ORIENTED_EDGE('',*,*,#1038,.T.);
#1322=ORIENTED_EDGE('',*,*,#1042,.F.);
#1323=ORIENTED_EDGE('',*,*,#1043,.T.);
#1324=ORIENTED_EDGE('',*,*,#1044,.F.);
#1325=ORIENTED_EDGE('',*,*,#1045,.F.);
#1326=ORIENTED_EDGE('',*,*,#1043,.F.);
#1327=ORIENTED_EDGE('',*,*,#1046,.F.);
#1328=ORIENTED_EDGE('',*,*,#1047,.F.);
#1329=ORIENTED_EDGE('',*,*,#1048,.T.);
#1330=ORIENTED_EDGE('',*,*,#1049,.F.);
#1331=ORIENTED_EDGE('',*,*,#1048,.F.);
#1332=ORIENTED_EDGE('',*,*,#1046,.T.);
#1333=ORIENTED_EDGE('',*,*,#1047,.T.);
#1334=ORIENTED_EDGE('',*,*,#1050,.T.);
#1335=ORIENTED_EDGE('',*,*,#1044,.T.);
#1336=ORIENTED_EDGE('',*,*,#1045,.T.);
#1337=ORIENTED_EDGE('',*,*,#1050,.F.);
#1338=ORIENTED_EDGE('',*,*,#1051,.F.);
#1339=ORIENTED_EDGE('',*,*,#1052,.T.);
#1340=ORIENTED_EDGE('',*,*,#1053,.F.);
#1341=ORIENTED_EDGE('',*,*,#1054,.F.);
#1342=ORIENTED_EDGE('',*,*,#1055,.F.);
#1343=ORIENTED_EDGE('',*,*,#1056,.T.);
#1344=ORIENTED_EDGE('',*,*,#1057,.F.);
#1345=ORIENTED_EDGE('',*,*,#1058,.F.);
#1346=ORIENTED_EDGE('',*,*,#1042,.T.);
#1347=ORIENTED_EDGE('',*,*,#1049,.T.);
#1348=ORIENTED_EDGE('',*,*,#1055,.T.);
#1349=ORIENTED_EDGE('',*,*,#1059,.F.);
#1350=ORIENTED_EDGE('',*,*,#1057,.T.);
#1351=ORIENTED_EDGE('',*,*,#1060,.T.);
#1352=ORIENTED_EDGE('',*,*,#1060,.F.);
#1353=ORIENTED_EDGE('',*,*,#1056,.F.);
#1354=ORIENTED_EDGE('',*,*,#1059,.T.);
#1355=ORIENTED_EDGE('',*,*,#1058,.T.);
#1356=ORIENTED_EDGE('',*,*,#1053,.T.);
#1357=ORIENTED_EDGE('',*,*,#1061,.T.);
#1358=ORIENTED_EDGE('',*,*,#1051,.T.);
#1359=ORIENTED_EDGE('',*,*,#1062,.F.);
#1360=ORIENTED_EDGE('',*,*,#1061,.F.);
#1361=ORIENTED_EDGE('',*,*,#1052,.F.);
#1362=ORIENTED_EDGE('',*,*,#1062,.T.);
#1363=ORIENTED_EDGE('',*,*,#1054,.T.);
#1364=ORIENTED_EDGE('',*,*,#1063,.F.);
#1365=ORIENTED_EDGE('',*,*,#1064,.T.);
#1366=ORIENTED_EDGE('',*,*,#1065,.T.);
#1367=ORIENTED_EDGE('',*,*,#1066,.T.);
#1368=ORIENTED_EDGE('',*,*,#1064,.F.);
#1369=ORIENTED_EDGE('',*,*,#1067,.T.);
#1370=ORIENTED_EDGE('',*,*,#1068,.T.);
#1371=ORIENTED_EDGE('',*,*,#1069,.T.);
#1372=ORIENTED_EDGE('',*,*,#1068,.F.);
#1373=ORIENTED_EDGE('',*,*,#1070,.F.);
#1374=ORIENTED_EDGE('',*,*,#1071,.T.);
#1375=ORIENTED_EDGE('',*,*,#1072,.T.);
#1376=ORIENTED_EDGE('',*,*,#1071,.F.);
#1377=ORIENTED_EDGE('',*,*,#1072,.F.);
#1378=ORIENTED_EDGE('',*,*,#1073,.T.);
#1379=ORIENTED_EDGE('',*,*,#1074,.T.);
#1380=ORIENTED_EDGE('',*,*,#1073,.F.);
#1381=ORIENTED_EDGE('',*,*,#1075,.F.);
#1382=ORIENTED_EDGE('',*,*,#1076,.T.);
#1383=ORIENTED_EDGE('',*,*,#1077,.T.);
#1384=ORIENTED_EDGE('',*,*,#1076,.F.);
#1385=ORIENTED_EDGE('',*,*,#1077,.F.);
#1386=ORIENTED_EDGE('',*,*,#1078,.T.);
#1387=ORIENTED_EDGE('',*,*,#1079,.T.);
#1388=ORIENTED_EDGE('',*,*,#1078,.F.);
#1389=ORIENTED_EDGE('',*,*,#1080,.F.);
#1390=ORIENTED_EDGE('',*,*,#1081,.T.);
#1391=ORIENTED_EDGE('',*,*,#1082,.T.);
#1392=ORIENTED_EDGE('',*,*,#1081,.F.);
#1393=ORIENTED_EDGE('',*,*,#1082,.F.);
#1394=ORIENTED_EDGE('',*,*,#1083,.T.);
#1395=ORIENTED_EDGE('',*,*,#1084,.T.);
#1396=ORIENTED_EDGE('',*,*,#1083,.F.);
#1397=ORIENTED_EDGE('',*,*,#1085,.F.);
#1398=ORIENTED_EDGE('',*,*,#1086,.T.);
#1399=ORIENTED_EDGE('',*,*,#1087,.T.);
#1400=ORIENTED_EDGE('',*,*,#1086,.F.);
#1401=ORIENTED_EDGE('',*,*,#1087,.F.);
#1402=ORIENTED_EDGE('',*,*,#1088,.T.);
#1403=ORIENTED_EDGE('',*,*,#1063,.T.);
#1404=ORIENTED_EDGE('',*,*,#1088,.F.);
#1405=ORIENTED_EDGE('',*,*,#1089,.T.);
#1406=ORIENTED_EDGE('',*,*,#1090,.T.);
#1407=ORIENTED_EDGE('',*,*,#1065,.F.);
#1408=ORIENTED_EDGE('',*,*,#1066,.F.);
#1409=ORIENTED_EDGE('',*,*,#1090,.F.);
#1410=ORIENTED_EDGE('',*,*,#1091,.T.);
#1411=ORIENTED_EDGE('',*,*,#1089,.F.);
#1412=ORIENTED_EDGE('',*,*,#1092,.T.);
#1413=ORIENTED_EDGE('',*,*,#1093,.T.);
#1414=ORIENTED_EDGE('',*,*,#1092,.F.);
#1415=ORIENTED_EDGE('',*,*,#1091,.F.);
#1416=ORIENTED_EDGE('',*,*,#1094,.F.);
#1417=ORIENTED_EDGE('',*,*,#1095,.T.);
#1418=ORIENTED_EDGE('',*,*,#1096,.T.);
#1419=ORIENTED_EDGE('',*,*,#1095,.F.);
#1420=ORIENTED_EDGE('',*,*,#1096,.F.);
#1421=ORIENTED_EDGE('',*,*,#1097,.T.);
#1422=ORIENTED_EDGE('',*,*,#1098,.T.);
#1423=ORIENTED_EDGE('',*,*,#1097,.F.);
#1424=ORIENTED_EDGE('',*,*,#1075,.T.);
#1425=ORIENTED_EDGE('',*,*,#1069,.F.);
#1426=ORIENTED_EDGE('',*,*,#1074,.F.);
#1427=ORIENTED_EDGE('',*,*,#1067,.F.);
#1428=ORIENTED_EDGE('',*,*,#1098,.F.);
#1429=ORIENTED_EDGE('',*,*,#1070,.T.);
#1430=ORIENTED_EDGE('',*,*,#1093,.F.);
#1431=ORIENTED_EDGE('',*,*,#1094,.T.);
#1432=ORIENTED_EDGE('',*,*,#1085,.T.);
#1433=ORIENTED_EDGE('',*,*,#1084,.F.);
#1434=ORIENTED_EDGE('',*,*,#1080,.T.);
#1435=ORIENTED_EDGE('',*,*,#1079,.F.);
#1436=ORIENTED_EDGE('',*,*,#1099,.F.);
#1437=ORIENTED_EDGE('',*,*,#1100,.T.);
#1438=ORIENTED_EDGE('',*,*,#1101,.T.);
#1439=ORIENTED_EDGE('',*,*,#1100,.F.);
#1440=ORIENTED_EDGE('',*,*,#1102,.F.);
#1441=ORIENTED_EDGE('',*,*,#1103,.T.);
#1442=ORIENTED_EDGE('',*,*,#1104,.T.);
#1443=ORIENTED_EDGE('',*,*,#1103,.F.);
#1444=ORIENTED_EDGE('',*,*,#1102,.T.);
#1445=ORIENTED_EDGE('',*,*,#1101,.F.);
#1446=ORIENTED_EDGE('',*,*,#1104,.F.);
#1447=ORIENTED_EDGE('',*,*,#1099,.T.);
#1448=ORIENTED_EDGE('',*,*,#1105,.F.);
#1449=ORIENTED_EDGE('',*,*,#1106,.T.);
#1450=ORIENTED_EDGE('',*,*,#1107,.T.);
#1451=ORIENTED_EDGE('',*,*,#1106,.F.);
#1452=ORIENTED_EDGE('',*,*,#1108,.T.);
#1453=ORIENTED_EDGE('',*,*,#1109,.T.);
#1454=ORIENTED_EDGE('',*,*,#1110,.T.);
#1455=ORIENTED_EDGE('',*,*,#1109,.F.);
#1456=ORIENTED_EDGE('',*,*,#1111,.T.);
#1457=ORIENTED_EDGE('',*,*,#1112,.T.);
#1458=ORIENTED_EDGE('',*,*,#1113,.T.);
#1459=ORIENTED_EDGE('',*,*,#1112,.F.);
#1460=ORIENTED_EDGE('',*,*,#1114,.T.);
#1461=ORIENTED_EDGE('',*,*,#1115,.T.);
#1462=ORIENTED_EDGE('',*,*,#1116,.T.);
#1463=ORIENTED_EDGE('',*,*,#1115,.F.);
#1464=ORIENTED_EDGE('',*,*,#1117,.T.);
#1465=ORIENTED_EDGE('',*,*,#1118,.F.);
#1466=ORIENTED_EDGE('',*,*,#1119,.T.);
#1467=ORIENTED_EDGE('',*,*,#1120,.F.);
#1468=ORIENTED_EDGE('',*,*,#1108,.F.);
#1469=ORIENTED_EDGE('',*,*,#1111,.F.);
#1470=ORIENTED_EDGE('',*,*,#1114,.F.);
#1471=ORIENTED_EDGE('',*,*,#1121,.T.);
#1472=ORIENTED_EDGE('',*,*,#1122,.F.);
#1473=ORIENTED_EDGE('',*,*,#1123,.F.);
#1474=ORIENTED_EDGE('',*,*,#1124,.T.);
#1475=ORIENTED_EDGE('',*,*,#1107,.F.);
#1476=ORIENTED_EDGE('',*,*,#1125,.T.);
#1477=ORIENTED_EDGE('',*,*,#1126,.F.);
#1478=ORIENTED_EDGE('',*,*,#1127,.F.);
#1479=ORIENTED_EDGE('',*,*,#1128,.T.);
#1480=ORIENTED_EDGE('',*,*,#1119,.F.);
#1481=ORIENTED_EDGE('',*,*,#1129,.F.);
#1482=ORIENTED_EDGE('',*,*,#1130,.F.);
#1483=ORIENTED_EDGE('',*,*,#1122,.T.);
#1484=ORIENTED_EDGE('',*,*,#1131,.T.);
#1485=ORIENTED_EDGE('',*,*,#1132,.F.);
#1486=ORIENTED_EDGE('',*,*,#1133,.F.);
#1487=ORIENTED_EDGE('',*,*,#1126,.T.);
#1488=ORIENTED_EDGE('',*,*,#1134,.T.);
#1489=ORIENTED_EDGE('',*,*,#1124,.F.);
#1490=ORIENTED_EDGE('',*,*,#1135,.F.);
#1491=ORIENTED_EDGE('',*,*,#1136,.T.);
#1492=ORIENTED_EDGE('',*,*,#1117,.F.);
#1493=ORIENTED_EDGE('',*,*,#1137,.F.);
#1494=ORIENTED_EDGE('',*,*,#1138,.F.);
#1495=ORIENTED_EDGE('',*,*,#1132,.T.);
#1496=ORIENTED_EDGE('',*,*,#1121,.F.);
#1497=ORIENTED_EDGE('',*,*,#1134,.F.);
#1498=ORIENTED_EDGE('',*,*,#1131,.F.);
#1499=ORIENTED_EDGE('',*,*,#1125,.F.);
#1500=ORIENTED_EDGE('',*,*,#1110,.F.);
#1501=ORIENTED_EDGE('',*,*,#1113,.F.);
#1502=ORIENTED_EDGE('',*,*,#1116,.F.);
#1503=ORIENTED_EDGE('',*,*,#1120,.T.);
#1504=ORIENTED_EDGE('',*,*,#1128,.F.);
#1505=ORIENTED_EDGE('',*,*,#1139,.F.);
#1506=ORIENTED_EDGE('',*,*,#1137,.T.);
#1507=ORIENTED_EDGE('',*,*,#1133,.T.);
#1508=ORIENTED_EDGE('',*,*,#1138,.T.);
#1509=ORIENTED_EDGE('',*,*,#1139,.T.);
#1510=ORIENTED_EDGE('',*,*,#1127,.T.);
#1511=ORIENTED_EDGE('',*,*,#1118,.T.);
#1512=ORIENTED_EDGE('',*,*,#1136,.F.);
#1513=ORIENTED_EDGE('',*,*,#1140,.F.);
#1514=ORIENTED_EDGE('',*,*,#1129,.T.);
#1515=ORIENTED_EDGE('',*,*,#1105,.T.);
#1516=ORIENTED_EDGE('',*,*,#1123,.T.);
#1517=ORIENTED_EDGE('',*,*,#1130,.T.);
#1518=ORIENTED_EDGE('',*,*,#1140,.T.);
#1519=ORIENTED_EDGE('',*,*,#1135,.T.);
#1520=ORIENTED_EDGE('',*,*,#1141,.T.);
#1521=ORIENTED_EDGE('',*,*,#1142,.T.);
#1522=ORIENTED_EDGE('',*,*,#1143,.F.);
#1523=ORIENTED_EDGE('',*,*,#1142,.F.);
#1524=ORIENTED_EDGE('',*,*,#1144,.T.);
#1525=ORIENTED_EDGE('',*,*,#1145,.T.);
#1526=ORIENTED_EDGE('',*,*,#1146,.F.);
#1527=ORIENTED_EDGE('',*,*,#1145,.F.);
#1528=ORIENTED_EDGE('',*,*,#1147,.T.);
#1529=ORIENTED_EDGE('',*,*,#1148,.T.);
#1530=ORIENTED_EDGE('',*,*,#1149,.T.);
#1531=ORIENTED_EDGE('',*,*,#1150,.T.);
#1532=ORIENTED_EDGE('',*,*,#1141,.F.);
#1533=ORIENTED_EDGE('',*,*,#1144,.F.);
#1534=ORIENTED_EDGE('',*,*,#1151,.F.);
#1535=ORIENTED_EDGE('',*,*,#1152,.F.);
#1536=ORIENTED_EDGE('',*,*,#1153,.F.);
#1537=ORIENTED_EDGE('',*,*,#1154,.F.);
#1538=ORIENTED_EDGE('',*,*,#1143,.T.);
#1539=ORIENTED_EDGE('',*,*,#1146,.T.);
#1540=ORIENTED_EDGE('',*,*,#1151,.T.);
#1541=ORIENTED_EDGE('',*,*,#1155,.F.);
#1542=ORIENTED_EDGE('',*,*,#1147,.F.);
#1543=ORIENTED_EDGE('',*,*,#1156,.T.);
#1544=ORIENTED_EDGE('',*,*,#1154,.T.);
#1545=ORIENTED_EDGE('',*,*,#1157,.F.);
#1546=ORIENTED_EDGE('',*,*,#1148,.F.);
#1547=ORIENTED_EDGE('',*,*,#1155,.T.);
#1548=ORIENTED_EDGE('',*,*,#1153,.T.);
#1549=ORIENTED_EDGE('',*,*,#1158,.F.);
#1550=ORIENTED_EDGE('',*,*,#1149,.F.);
#1551=ORIENTED_EDGE('',*,*,#1157,.T.);
#1552=ORIENTED_EDGE('',*,*,#1152,.T.);
#1553=ORIENTED_EDGE('',*,*,#1156,.F.);
#1554=ORIENTED_EDGE('',*,*,#1150,.F.);
#1555=ORIENTED_EDGE('',*,*,#1158,.T.);
#1556=ORIENTED_EDGE('',*,*,#1159,.F.);
#1557=ORIENTED_EDGE('',*,*,#1160,.F.);
#1558=ORIENTED_EDGE('',*,*,#1161,.T.);
#1559=ORIENTED_EDGE('',*,*,#1162,.T.);
#1560=ORIENTED_EDGE('',*,*,#1163,.F.);
#1561=ORIENTED_EDGE('',*,*,#1164,.F.);
#1562=ORIENTED_EDGE('',*,*,#1159,.T.);
#1563=ORIENTED_EDGE('',*,*,#1165,.T.);
#1564=ORIENTED_EDGE('',*,*,#1166,.F.);
#1565=ORIENTED_EDGE('',*,*,#1167,.F.);
#1566=ORIENTED_EDGE('',*,*,#1163,.T.);
#1567=ORIENTED_EDGE('',*,*,#1168,.T.);
#1568=ORIENTED_EDGE('',*,*,#1169,.F.);
#1569=ORIENTED_EDGE('',*,*,#1170,.F.);
#1570=ORIENTED_EDGE('',*,*,#1166,.T.);
#1571=ORIENTED_EDGE('',*,*,#1171,.T.);
#1572=ORIENTED_EDGE('',*,*,#1172,.F.);
#1573=ORIENTED_EDGE('',*,*,#1173,.F.);
#1574=ORIENTED_EDGE('',*,*,#1169,.T.);
#1575=ORIENTED_EDGE('',*,*,#1174,.T.);
#1576=ORIENTED_EDGE('',*,*,#1175,.F.);
#1577=ORIENTED_EDGE('',*,*,#1176,.F.);
#1578=ORIENTED_EDGE('',*,*,#1172,.T.);
#1579=ORIENTED_EDGE('',*,*,#1177,.T.);
#1580=ORIENTED_EDGE('',*,*,#1178,.F.);
#1581=ORIENTED_EDGE('',*,*,#1179,.F.);
#1582=ORIENTED_EDGE('',*,*,#1175,.T.);
#1583=ORIENTED_EDGE('',*,*,#1180,.T.);
#1584=ORIENTED_EDGE('',*,*,#1181,.F.);
#1585=ORIENTED_EDGE('',*,*,#1182,.F.);
#1586=ORIENTED_EDGE('',*,*,#1178,.T.);
#1587=ORIENTED_EDGE('',*,*,#1183,.T.);
#1588=ORIENTED_EDGE('',*,*,#1184,.F.);
#1589=ORIENTED_EDGE('',*,*,#1185,.F.);
#1590=ORIENTED_EDGE('',*,*,#1181,.T.);
#1591=ORIENTED_EDGE('',*,*,#1186,.T.);
#1592=ORIENTED_EDGE('',*,*,#1187,.F.);
#1593=ORIENTED_EDGE('',*,*,#1188,.F.);
#1594=ORIENTED_EDGE('',*,*,#1184,.T.);
#1595=ORIENTED_EDGE('',*,*,#1189,.T.);
#1596=ORIENTED_EDGE('',*,*,#1190,.F.);
#1597=ORIENTED_EDGE('',*,*,#1191,.F.);
#1598=ORIENTED_EDGE('',*,*,#1187,.T.);
#1599=ORIENTED_EDGE('',*,*,#1192,.T.);
#1600=ORIENTED_EDGE('',*,*,#1193,.F.);
#1601=ORIENTED_EDGE('',*,*,#1194,.F.);
#1602=ORIENTED_EDGE('',*,*,#1190,.T.);
#1603=ORIENTED_EDGE('',*,*,#1195,.T.);
#1604=ORIENTED_EDGE('',*,*,#1196,.F.);
#1605=ORIENTED_EDGE('',*,*,#1197,.F.);
#1606=ORIENTED_EDGE('',*,*,#1193,.T.);
#1607=ORIENTED_EDGE('',*,*,#1198,.T.);
#1608=ORIENTED_EDGE('',*,*,#1199,.F.);
#1609=ORIENTED_EDGE('',*,*,#1200,.F.);
#1610=ORIENTED_EDGE('',*,*,#1201,.T.);
#1611=ORIENTED_EDGE('',*,*,#1202,.T.);
#1612=ORIENTED_EDGE('',*,*,#1203,.T.);
#1613=ORIENTED_EDGE('',*,*,#1204,.T.);
#1614=ORIENTED_EDGE('',*,*,#1202,.F.);
#1615=ORIENTED_EDGE('',*,*,#1205,.T.);
#1616=ORIENTED_EDGE('',*,*,#1206,.T.);
#1617=ORIENTED_EDGE('',*,*,#1207,.F.);
#1618=ORIENTED_EDGE('',*,*,#1208,.F.);
#1619=ORIENTED_EDGE('',*,*,#1199,.T.);
#1620=ORIENTED_EDGE('',*,*,#1209,.T.);
#1621=ORIENTED_EDGE('',*,*,#1210,.F.);
#1622=ORIENTED_EDGE('',*,*,#1211,.F.);
#1623=ORIENTED_EDGE('',*,*,#1207,.T.);
#1624=ORIENTED_EDGE('',*,*,#1212,.T.);
#1625=ORIENTED_EDGE('',*,*,#1213,.F.);
#1626=ORIENTED_EDGE('',*,*,#1214,.F.);
#1627=ORIENTED_EDGE('',*,*,#1210,.T.);
#1628=ORIENTED_EDGE('',*,*,#1215,.T.);
#1629=ORIENTED_EDGE('',*,*,#1216,.F.);
#1630=ORIENTED_EDGE('',*,*,#1217,.F.);
#1631=ORIENTED_EDGE('',*,*,#1213,.T.);
#1632=ORIENTED_EDGE('',*,*,#1218,.T.);
#1633=ORIENTED_EDGE('',*,*,#1219,.F.);
#1634=ORIENTED_EDGE('',*,*,#1220,.F.);
#1635=ORIENTED_EDGE('',*,*,#1216,.T.);
#1636=ORIENTED_EDGE('',*,*,#1221,.T.);
#1637=ORIENTED_EDGE('',*,*,#1222,.F.);
#1638=ORIENTED_EDGE('',*,*,#1223,.F.);
#1639=ORIENTED_EDGE('',*,*,#1219,.T.);
#1640=ORIENTED_EDGE('',*,*,#1224,.T.);
#1641=ORIENTED_EDGE('',*,*,#1225,.F.);
#1642=ORIENTED_EDGE('',*,*,#1226,.F.);
#1643=ORIENTED_EDGE('',*,*,#1222,.T.);
#1644=ORIENTED_EDGE('',*,*,#1227,.T.);
#1645=ORIENTED_EDGE('',*,*,#1228,.F.);
#1646=ORIENTED_EDGE('',*,*,#1229,.F.);
#1647=ORIENTED_EDGE('',*,*,#1225,.T.);
#1648=ORIENTED_EDGE('',*,*,#1230,.T.);
#1649=ORIENTED_EDGE('',*,*,#1231,.F.);
#1650=ORIENTED_EDGE('',*,*,#1232,.F.);
#1651=ORIENTED_EDGE('',*,*,#1228,.T.);
#1652=ORIENTED_EDGE('',*,*,#1233,.T.);
#1653=ORIENTED_EDGE('',*,*,#1234,.F.);
#1654=ORIENTED_EDGE('',*,*,#1235,.F.);
#1655=ORIENTED_EDGE('',*,*,#1231,.T.);
#1656=ORIENTED_EDGE('',*,*,#1236,.T.);
#1657=ORIENTED_EDGE('',*,*,#1237,.F.);
#1658=ORIENTED_EDGE('',*,*,#1238,.F.);
#1659=ORIENTED_EDGE('',*,*,#1234,.T.);
#1660=ORIENTED_EDGE('',*,*,#1239,.T.);
#1661=ORIENTED_EDGE('',*,*,#1240,.F.);
#1662=ORIENTED_EDGE('',*,*,#1241,.F.);
#1663=ORIENTED_EDGE('',*,*,#1237,.T.);
#1664=ORIENTED_EDGE('',*,*,#1242,.T.);
#1665=ORIENTED_EDGE('',*,*,#1243,.F.);
#1666=ORIENTED_EDGE('',*,*,#1244,.F.);
#1667=ORIENTED_EDGE('',*,*,#1245,.T.);
#1668=ORIENTED_EDGE('',*,*,#1246,.T.);
#1669=ORIENTED_EDGE('',*,*,#1247,.T.);
#1670=ORIENTED_EDGE('',*,*,#1248,.T.);
#1671=ORIENTED_EDGE('',*,*,#1249,.T.);
#1672=ORIENTED_EDGE('',*,*,#1250,.F.);
#1673=ORIENTED_EDGE('',*,*,#1249,.F.);
#1674=ORIENTED_EDGE('',*,*,#1251,.T.);
#1675=ORIENTED_EDGE('',*,*,#1252,.T.);
#1676=ORIENTED_EDGE('',*,*,#1253,.F.);
#1677=ORIENTED_EDGE('',*,*,#1254,.T.);
#1678=ORIENTED_EDGE('',*,*,#1203,.F.);
#1679=ORIENTED_EDGE('',*,*,#1204,.F.);
#1680=ORIENTED_EDGE('',*,*,#1254,.F.);
#1681=ORIENTED_EDGE('',*,*,#1255,.F.);
#1682=ORIENTED_EDGE('',*,*,#1256,.T.);
#1683=ORIENTED_EDGE('',*,*,#1257,.F.);
#1684=ORIENTED_EDGE('',*,*,#1256,.F.);
#1685=ORIENTED_EDGE('',*,*,#1257,.T.);
#1686=ORIENTED_EDGE('',*,*,#1258,.T.);
#1687=ORIENTED_EDGE('',*,*,#1253,.T.);
#1688=ORIENTED_EDGE('',*,*,#1258,.F.);
#1689=ORIENTED_EDGE('',*,*,#1243,.T.);
#1690=ORIENTED_EDGE('',*,*,#1259,.T.);
#1691=ORIENTED_EDGE('',*,*,#1260,.F.);
#1692=ORIENTED_EDGE('',*,*,#1240,.T.);
#1693=ORIENTED_EDGE('',*,*,#1261,.T.);
#1694=ORIENTED_EDGE('',*,*,#1262,.T.);
#1695=ORIENTED_EDGE('',*,*,#1244,.T.);
#1696=ORIENTED_EDGE('',*,*,#1260,.T.);
#1697=ORIENTED_EDGE('',*,*,#1263,.F.);
#1698=ORIENTED_EDGE('',*,*,#1162,.F.);
#1699=ORIENTED_EDGE('',*,*,#1264,.T.);
#1700=ORIENTED_EDGE('',*,*,#1200,.T.);
#1701=ORIENTED_EDGE('',*,*,#1208,.T.);
#1702=ORIENTED_EDGE('',*,*,#1211,.T.);
#1703=ORIENTED_EDGE('',*,*,#1214,.T.);
#1704=ORIENTED_EDGE('',*,*,#1217,.T.);
#1705=ORIENTED_EDGE('',*,*,#1220,.T.);
#1706=ORIENTED_EDGE('',*,*,#1223,.T.);
#1707=ORIENTED_EDGE('',*,*,#1226,.T.);
#1708=ORIENTED_EDGE('',*,*,#1229,.T.);
#1709=ORIENTED_EDGE('',*,*,#1232,.T.);
#1710=ORIENTED_EDGE('',*,*,#1235,.T.);
#1711=ORIENTED_EDGE('',*,*,#1238,.T.);
#1712=ORIENTED_EDGE('',*,*,#1241,.T.);
#1713=ORIENTED_EDGE('',*,*,#1263,.T.);
#1714=ORIENTED_EDGE('',*,*,#1259,.F.);
#1715=ORIENTED_EDGE('',*,*,#1252,.F.);
#1716=ORIENTED_EDGE('',*,*,#1265,.F.);
#1717=ORIENTED_EDGE('',*,*,#1198,.F.);
#1718=ORIENTED_EDGE('',*,*,#1195,.F.);
#1719=ORIENTED_EDGE('',*,*,#1192,.F.);
#1720=ORIENTED_EDGE('',*,*,#1189,.F.);
#1721=ORIENTED_EDGE('',*,*,#1186,.F.);
#1722=ORIENTED_EDGE('',*,*,#1183,.F.);
#1723=ORIENTED_EDGE('',*,*,#1180,.F.);
#1724=ORIENTED_EDGE('',*,*,#1177,.F.);
#1725=ORIENTED_EDGE('',*,*,#1174,.F.);
#1726=ORIENTED_EDGE('',*,*,#1171,.F.);
#1727=ORIENTED_EDGE('',*,*,#1168,.F.);
#1728=ORIENTED_EDGE('',*,*,#1165,.F.);
#1729=ORIENTED_EDGE('',*,*,#1196,.T.);
#1730=ORIENTED_EDGE('',*,*,#1265,.T.);
#1731=ORIENTED_EDGE('',*,*,#1251,.F.);
#1732=ORIENTED_EDGE('',*,*,#1248,.F.);
#1733=ORIENTED_EDGE('',*,*,#1266,.F.);
#1734=ORIENTED_EDGE('',*,*,#1206,.F.);
#1735=ORIENTED_EDGE('',*,*,#1267,.T.);
#1736=ORIENTED_EDGE('',*,*,#1160,.T.);
#1737=ORIENTED_EDGE('',*,*,#1164,.T.);
#1738=ORIENTED_EDGE('',*,*,#1167,.T.);
#1739=ORIENTED_EDGE('',*,*,#1170,.T.);
#1740=ORIENTED_EDGE('',*,*,#1173,.T.);
#1741=ORIENTED_EDGE('',*,*,#1176,.T.);
#1742=ORIENTED_EDGE('',*,*,#1179,.T.);
#1743=ORIENTED_EDGE('',*,*,#1182,.T.);
#1744=ORIENTED_EDGE('',*,*,#1185,.T.);
#1745=ORIENTED_EDGE('',*,*,#1188,.T.);
#1746=ORIENTED_EDGE('',*,*,#1191,.T.);
#1747=ORIENTED_EDGE('',*,*,#1194,.T.);
#1748=ORIENTED_EDGE('',*,*,#1197,.T.);
#1749=ORIENTED_EDGE('',*,*,#1266,.T.);
#1750=ORIENTED_EDGE('',*,*,#1247,.F.);
#1751=ORIENTED_EDGE('',*,*,#1246,.F.);
#1752=ORIENTED_EDGE('',*,*,#1245,.F.);
#1753=ORIENTED_EDGE('',*,*,#1262,.F.);
#1754=ORIENTED_EDGE('',*,*,#1261,.F.);
#1755=ORIENTED_EDGE('',*,*,#1242,.F.);
#1756=ORIENTED_EDGE('',*,*,#1239,.F.);
#1757=ORIENTED_EDGE('',*,*,#1236,.F.);
#1758=ORIENTED_EDGE('',*,*,#1233,.F.);
#1759=ORIENTED_EDGE('',*,*,#1230,.F.);
#1760=ORIENTED_EDGE('',*,*,#1227,.F.);
#1761=ORIENTED_EDGE('',*,*,#1224,.F.);
#1762=ORIENTED_EDGE('',*,*,#1221,.F.);
#1763=ORIENTED_EDGE('',*,*,#1218,.F.);
#1764=ORIENTED_EDGE('',*,*,#1215,.F.);
#1765=ORIENTED_EDGE('',*,*,#1212,.F.);
#1766=ORIENTED_EDGE('',*,*,#1209,.F.);
#1767=ORIENTED_EDGE('',*,*,#1250,.T.);
#1768=ORIENTED_EDGE('',*,*,#1264,.F.);
#1769=ORIENTED_EDGE('',*,*,#1161,.F.);
#1770=ORIENTED_EDGE('',*,*,#1267,.F.);
#1771=ORIENTED_EDGE('',*,*,#1205,.F.);
#1772=ORIENTED_EDGE('',*,*,#1201,.F.);
#1773=ORIENTED_EDGE('',*,*,#1255,.T.);
#1774=ORIENTED_EDGE('',*,*,#1268,.T.);
#1775=ORIENTED_EDGE('',*,*,#1269,.T.);
#1776=ORIENTED_EDGE('',*,*,#1270,.T.);
#1777=ORIENTED_EDGE('',*,*,#1271,.T.);
#1778=ORIENTED_EDGE('',*,*,#1272,.T.);
#1779=ORIENTED_EDGE('',*,*,#1273,.T.);
#1780=ORIENTED_EDGE('',*,*,#1274,.T.);
#1781=ORIENTED_EDGE('',*,*,#1275,.T.);
#1782=ORIENTED_EDGE('',*,*,#1276,.F.);
#1783=ORIENTED_EDGE('',*,*,#1277,.F.);
#1784=ORIENTED_EDGE('',*,*,#1278,.T.);
#1785=ORIENTED_EDGE('',*,*,#1279,.T.);
#1786=ORIENTED_EDGE('',*,*,#1274,.F.);
#1787=ORIENTED_EDGE('',*,*,#1280,.F.);
#1788=ORIENTED_EDGE('',*,*,#1281,.T.);
#1789=ORIENTED_EDGE('',*,*,#1282,.T.);
#1790=ORIENTED_EDGE('',*,*,#1278,.F.);
#1791=ORIENTED_EDGE('',*,*,#1283,.F.);
#1792=ORIENTED_EDGE('',*,*,#1284,.T.);
#1793=ORIENTED_EDGE('',*,*,#1285,.T.);
#1794=ORIENTED_EDGE('',*,*,#1281,.F.);
#1795=ORIENTED_EDGE('',*,*,#1286,.F.);
#1796=ORIENTED_EDGE('',*,*,#1287,.T.);
#1797=ORIENTED_EDGE('',*,*,#1288,.T.);
#1798=ORIENTED_EDGE('',*,*,#1284,.F.);
#1799=ORIENTED_EDGE('',*,*,#1289,.F.);
#1800=ORIENTED_EDGE('',*,*,#1276,.T.);
#1801=ORIENTED_EDGE('',*,*,#1290,.T.);
#1802=ORIENTED_EDGE('',*,*,#1287,.F.);
#1803=ORIENTED_EDGE('',*,*,#1291,.F.);
#1804=ORIENTED_EDGE('',*,*,#1292,.F.);
#1805=ORIENTED_EDGE('',*,*,#1272,.F.);
#1806=ORIENTED_EDGE('',*,*,#1293,.F.);
#1807=ORIENTED_EDGE('',*,*,#1279,.F.);
#1808=ORIENTED_EDGE('',*,*,#1293,.T.);
#1809=ORIENTED_EDGE('',*,*,#1271,.F.);
#1810=ORIENTED_EDGE('',*,*,#1294,.F.);
#1811=ORIENTED_EDGE('',*,*,#1275,.F.);
#1812=ORIENTED_EDGE('',*,*,#1292,.T.);
#1813=ORIENTED_EDGE('',*,*,#1282,.F.);
#1814=ORIENTED_EDGE('',*,*,#1295,.F.);
#1815=ORIENTED_EDGE('',*,*,#1273,.F.);
#1816=ORIENTED_EDGE('',*,*,#1294,.T.);
#1817=ORIENTED_EDGE('',*,*,#1270,.F.);
#1818=ORIENTED_EDGE('',*,*,#1296,.F.);
#1819=ORIENTED_EDGE('',*,*,#1290,.F.);
#1820=ORIENTED_EDGE('',*,*,#1295,.T.);
#1821=ORIENTED_EDGE('',*,*,#1285,.F.);
#1822=ORIENTED_EDGE('',*,*,#1297,.F.);
#1823=ORIENTED_EDGE('',*,*,#1268,.F.);
#1824=ORIENTED_EDGE('',*,*,#1296,.T.);
#1825=ORIENTED_EDGE('',*,*,#1269,.F.);
#1826=ORIENTED_EDGE('',*,*,#1297,.T.);
#1827=ORIENTED_EDGE('',*,*,#1288,.F.);
#1828=ORIENTED_EDGE('',*,*,#1277,.T.);
#1829=ORIENTED_EDGE('',*,*,#1298,.F.);
#1830=ORIENTED_EDGE('',*,*,#1299,.F.);
#1831=ORIENTED_EDGE('',*,*,#1300,.T.);
#1832=ORIENTED_EDGE('',*,*,#1280,.T.);
#1833=ORIENTED_EDGE('',*,*,#1300,.F.);
#1834=ORIENTED_EDGE('',*,*,#1301,.F.);
#1835=ORIENTED_EDGE('',*,*,#1302,.T.);
#1836=ORIENTED_EDGE('',*,*,#1283,.T.);
#1837=ORIENTED_EDGE('',*,*,#1302,.F.);
#1838=ORIENTED_EDGE('',*,*,#1303,.F.);
#1839=ORIENTED_EDGE('',*,*,#1304,.T.);
#1840=ORIENTED_EDGE('',*,*,#1286,.T.);
#1841=ORIENTED_EDGE('',*,*,#1304,.F.);
#1842=ORIENTED_EDGE('',*,*,#1305,.F.);
#1843=ORIENTED_EDGE('',*,*,#1306,.T.);
#1844=ORIENTED_EDGE('',*,*,#1289,.T.);
#1845=ORIENTED_EDGE('',*,*,#1306,.F.);
#1846=ORIENTED_EDGE('',*,*,#1307,.F.);
#1847=ORIENTED_EDGE('',*,*,#1308,.T.);
#1848=ORIENTED_EDGE('',*,*,#1291,.T.);
#1849=ORIENTED_EDGE('',*,*,#1308,.F.);
#1850=ORIENTED_EDGE('',*,*,#1309,.F.);
#1851=ORIENTED_EDGE('',*,*,#1298,.T.);
#1852=ORIENTED_EDGE('',*,*,#1299,.T.);
#1853=ORIENTED_EDGE('',*,*,#1309,.T.);
#1854=ORIENTED_EDGE('',*,*,#1307,.T.);
#1855=ORIENTED_EDGE('',*,*,#1305,.T.);
#1856=ORIENTED_EDGE('',*,*,#1303,.T.);
#1857=ORIENTED_EDGE('',*,*,#1301,.T.);
#1858=CYLINDRICAL_SURFACE('',#2109,7.);
#1859=CYLINDRICAL_SURFACE('',#2112,9.);
#1860=CYLINDRICAL_SURFACE('',#2128,7.);
#1861=CYLINDRICAL_SURFACE('',#2147,9.);
#1862=CYLINDRICAL_SURFACE('',#2154,14.0000000000046);
#1863=CYLINDRICAL_SURFACE('',#2156,13.9999999999978);
#1864=CYLINDRICAL_SURFACE('',#2166,35.9999999999978);
#1865=CYLINDRICAL_SURFACE('',#2168,48.0000000000047);
#1866=CYLINDRICAL_SURFACE('',#2175,48.0000000000047);
#1867=CYLINDRICAL_SURFACE('',#2177,36.0000000000017);
#1868=CYLINDRICAL_SURFACE('',#2190,7.);
#1869=CYLINDRICAL_SURFACE('',#2193,12.);
#1870=CYLINDRICAL_SURFACE('',#2199,4.);
#1871=CYLINDRICAL_SURFACE('',#2202,1.64999999999999);
#1872=CYLINDRICAL_SURFACE('',#2205,1.64999999999999);
#1873=CYLINDRICAL_SURFACE('',#2208,7.);
#1874=CYLINDRICAL_SURFACE('',#2222,2.125);
#1875=CYLINDRICAL_SURFACE('',#2225,2.25);
#1876=CYLINDRICAL_SURFACE('',#2235,1.6211138875);
#1877=CYLINDRICAL_SURFACE('',#2237,1.6211138875);
#1878=CYLINDRICAL_SURFACE('',#2238,1.6211138875);
#1879=CYLINDRICAL_SURFACE('',#2239,1.6211138875);
#1880=CYLINDRICAL_SURFACE('',#2240,1.6211138875);
#1881=CYLINDRICAL_SURFACE('',#2241,1.6211138875);
#1882=CYLINDRICAL_SURFACE('',#2242,1.6211138875);
#1883=CYLINDRICAL_SURFACE('',#2243,1.6211138875);
#1884=CYLINDRICAL_SURFACE('',#2244,1.6211138875);
#1885=CYLINDRICAL_SURFACE('',#2245,1.6211138875);
#1886=CYLINDRICAL_SURFACE('',#2246,1.6211138875);
#1887=CYLINDRICAL_SURFACE('',#2247,1.6211138875);
#1888=CYLINDRICAL_SURFACE('',#2248,1.6211138875);
#1889=CYLINDRICAL_SURFACE('',#2249,2.);
#1890=CYLINDRICAL_SURFACE('',#2254,2.);
#1891=CYLINDRICAL_SURFACE('',#2255,2.);
#1892=CYLINDRICAL_SURFACE('',#2256,2.);
#1893=CYLINDRICAL_SURFACE('',#2257,2.);
#1894=CYLINDRICAL_SURFACE('',#2258,2.);
#1895=CYLINDRICAL_SURFACE('',#2259,2.);
#1896=CYLINDRICAL_SURFACE('',#2260,2.);
#1897=CYLINDRICAL_SURFACE('',#2261,2.);
#1898=CYLINDRICAL_SURFACE('',#2262,2.);
#1899=CYLINDRICAL_SURFACE('',#2263,2.);
#1900=CYLINDRICAL_SURFACE('',#2264,2.);
#1901=CYLINDRICAL_SURFACE('',#2265,2.);
#1902=CYLINDRICAL_SURFACE('',#2281,2.);
#1903=CYLINDRICAL_SURFACE('',#2282,1.6211138875);
#1904=ADVANCED_FACE('',(#252),#1858,.F.);
#1905=ADVANCED_FACE('',(#253),#1859,.T.);
#1906=ADVANCED_FACE('',(#254,#171),#196,.T.);
#1907=ADVANCED_FACE('',(#255,#172),#197,.F.);
#1908=ADVANCED_FACE('',(#256),#134,.T.);
#1909=ADVANCED_FACE('',(#257),#135,.T.);
#1910=ADVANCED_FACE('',(#258,#173,#174),#1860,.T.);
#1911=ADVANCED_FACE('',(#259),#198,.T.);
#1912=ADVANCED_FACE('',(#260),#199,.F.);
#1913=ADVANCED_FACE('',(#261),#200,.T.);
#1914=ADVANCED_FACE('',(#262),#201,.F.);
#1915=ADVANCED_FACE('',(#263),#202,.T.);
#1916=ADVANCED_FACE('',(#264),#203,.T.);
#1917=ADVANCED_FACE('',(#265),#204,.F.);
#1918=ADVANCED_FACE('',(#266),#205,.T.);
#1919=ADVANCED_FACE('',(#267),#136,.F.);
#1920=ADVANCED_FACE('',(#268),#1861,.F.);
#1921=ADVANCED_FACE('',(#269),#137,.F.);
#1922=ADVANCED_FACE('',(#270),#1862,.T.);
#1923=ADVANCED_FACE('',(#271),#1863,.T.);
#1924=ADVANCED_FACE('',(#272),#138,.F.);
#1925=ADVANCED_FACE('',(#273),#139,.F.);
#1926=ADVANCED_FACE('',(#274),#1864,.F.);
#1927=ADVANCED_FACE('',(#275),#1865,.T.);
#1928=ADVANCED_FACE('',(#276),#129,.T.);
#1929=ADVANCED_FACE('',(#277),#130,.T.);
#1930=ADVANCED_FACE('',(#278),#1866,.T.);
#1931=ADVANCED_FACE('',(#279),#1867,.F.);
#1932=ADVANCED_FACE('',(#280),#140,.F.);
#1933=ADVANCED_FACE('',(#281,#175),#206,.F.);
#1934=ADVANCED_FACE('',(#282,#176),#207,.F.);
#1935=ADVANCED_FACE('',(#283,#177),#208,.T.);
#1936=ADVANCED_FACE('',(#284,#178),#209,.T.);
#1937=ADVANCED_FACE('',(#285,#179),#210,.F.);
#1938=ADVANCED_FACE('',(#286,#180),#211,.F.);
#1939=ADVANCED_FACE('',(#287),#1868,.F.);
#1940=ADVANCED_FACE('',(#288),#1869,.T.);
#1941=ADVANCED_FACE('',(#289,#181),#212,.F.);
#1942=ADVANCED_FACE('',(#290,#182),#213,.T.);
#1943=ADVANCED_FACE('',(#291),#1870,.F.);
#1944=ADVANCED_FACE('',(#292),#1871,.F.);
#1945=ADVANCED_FACE('',(#293),#1872,.F.);
#1946=ADVANCED_FACE('',(#294),#1873,.F.);
#1947=ADVANCED_FACE('',(#295,#183,#184,#185),#214,.T.);
#1948=ADVANCED_FACE('',(#296,#186),#215,.F.);
#1949=ADVANCED_FACE('',(#297),#216,.F.);
#1950=ADVANCED_FACE('',(#298),#217,.F.);
#1951=ADVANCED_FACE('',(#299),#218,.F.);
#1952=ADVANCED_FACE('',(#300,#187,#188,#189),#219,.F.);
#1953=ADVANCED_FACE('',(#301),#220,.F.);
#1954=ADVANCED_FACE('',(#302),#221,.T.);
#1955=ADVANCED_FACE('',(#303,#190),#222,.F.);
#1956=ADVANCED_FACE('',(#304),#223,.F.);
#1957=ADVANCED_FACE('',(#305),#1874,.F.);
#1958=ADVANCED_FACE('',(#306),#1875,.F.);
#1959=ADVANCED_FACE('',(#307,#191,#192),#224,.T.);
#1960=ADVANCED_FACE('',(#308,#193,#194),#225,.F.);
#1961=ADVANCED_FACE('',(#309),#226,.F.);
#1962=ADVANCED_FACE('',(#310),#227,.F.);
#1963=ADVANCED_FACE('',(#311),#228,.F.);
#1964=ADVANCED_FACE('',(#312),#229,.F.);
#1965=ADVANCED_FACE('',(#313),#1876,.T.);
#1966=ADVANCED_FACE('',(#314),#1877,.T.);
#1967=ADVANCED_FACE('',(#315),#1878,.T.);
#1968=ADVANCED_FACE('',(#316),#1879,.T.);
#1969=ADVANCED_FACE('',(#317),#1880,.T.);
#1970=ADVANCED_FACE('',(#318),#1881,.T.);
#1971=ADVANCED_FACE('',(#319),#1882,.T.);
#1972=ADVANCED_FACE('',(#320),#1883,.T.);
#1973=ADVANCED_FACE('',(#321),#1884,.T.);
#1974=ADVANCED_FACE('',(#322),#1885,.T.);
#1975=ADVANCED_FACE('',(#323),#1886,.T.);
#1976=ADVANCED_FACE('',(#324),#1887,.T.);
#1977=ADVANCED_FACE('',(#325),#1888,.T.);
#1978=ADVANCED_FACE('',(#326),#1889,.T.);
#1979=ADVANCED_FACE('',(#327),#1890,.T.);
#1980=ADVANCED_FACE('',(#328),#1891,.T.);
#1981=ADVANCED_FACE('',(#329),#1892,.T.);
#1982=ADVANCED_FACE('',(#330),#1893,.T.);
#1983=ADVANCED_FACE('',(#331),#1894,.T.);
#1984=ADVANCED_FACE('',(#332),#1895,.T.);
#1985=ADVANCED_FACE('',(#333),#1896,.T.);
#1986=ADVANCED_FACE('',(#334),#1897,.T.);
#1987=ADVANCED_FACE('',(#335),#1898,.T.);
#1988=ADVANCED_FACE('',(#336),#1899,.T.);
#1989=ADVANCED_FACE('',(#337),#1900,.T.);
#1990=ADVANCED_FACE('',(#338),#1901,.T.);
#1991=ADVANCED_FACE('',(#339),#131,.T.);
#1992=ADVANCED_FACE('',(#340),#141,.F.);
#1993=ADVANCED_FACE('',(#341),#142,.T.);
#1994=ADVANCED_FACE('',(#342),#132,.T.);
#1995=ADVANCED_FACE('',(#343),#133,.T.);
#1996=ADVANCED_FACE('',(#344),#1902,.T.);
#1997=ADVANCED_FACE('',(#345),#63,.T.);
#1998=ADVANCED_FACE('',(#346),#1903,.T.);
#1999=ADVANCED_FACE('',(#347),#64,.T.);
#2000=ADVANCED_FACE('',(#348),#230,.F.);
#2001=ADVANCED_FACE('',(#349),#231,.F.);
#2002=ADVANCED_FACE('',(#350,#195),#232,.T.);
#2003=ADVANCED_FACE('',(#351),#233,.F.);
#2004=ADVANCED_FACE('',(#352),#234,.F.);
#2005=ADVANCED_FACE('',(#353),#235,.F.);
#2006=ADVANCED_FACE('',(#354),#236,.F.);
#2007=ADVANCED_FACE('',(#355),#237,.F.);
#2008=ADVANCED_FACE('',(#356),#238,.F.);
#2009=ADVANCED_FACE('',(#357),#239,.T.);
#2010=ADVANCED_FACE('',(#358),#240,.T.);
#2011=ADVANCED_FACE('',(#359),#241,.T.);
#2012=ADVANCED_FACE('',(#360),#242,.T.);
#2013=ADVANCED_FACE('',(#361),#243,.T.);
#2014=ADVANCED_FACE('',(#362),#244,.T.);
#2015=ADVANCED_FACE('',(#363),#245,.F.);
#2016=ADVANCED_FACE('',(#364),#246,.F.);
#2017=ADVANCED_FACE('',(#365),#247,.F.);
#2018=ADVANCED_FACE('',(#366),#248,.F.);
#2019=ADVANCED_FACE('',(#367),#249,.F.);
#2020=ADVANCED_FACE('',(#368),#250,.F.);
#2021=ADVANCED_FACE('',(#369),#251,.T.);
#2022=CLOSED_SHELL('',(#1904,#1905,#1906,#1907));
#2023=CLOSED_SHELL('',(#1908,#1909,#1910,#1911,#1912,#1913,#1914,#1915,
#1916,#1917,#1918));
#2024=CLOSED_SHELL('',(#1919,#1920,#1921,#1922,#1923,#1924,#1925,#1926,
#1927,#1928,#1929,#1930,#1931,#1932,#1933,#1934,#1935,#1936,#1937,#1938));
#2025=CLOSED_SHELL('',(#1939,#1940,#1941,#1942));
#2026=CLOSED_SHELL('',(#1943,#1944,#1945,#1946,#1947,#1948,#1949,#1950,
#1951,#1952,#1953,#1954,#1955,#1956));
#2027=CLOSED_SHELL('',(#1957,#1958,#1959,#1960,#1961,#1962,#1963,#1964));
#2028=CLOSED_SHELL('',(#1965,#1966,#1967,#1968,#1969,#1970,#1971,#1972,
#1973,#1974,#1975,#1976,#1977,#1978,#1979,#1980,#1981,#1982,#1983,#1984,
#1985,#1986,#1987,#1988,#1989,#1990,#1991,#1992,#1993,#1994,#1995,#1996,
#1997,#1998,#1999,#2000,#2001,#2002,#2003,#2004,#2005,#2006,#2007,#2008,
#2009,#2010,#2011,#2012,#2013,#2014,#2015,#2016,#2017,#2018,#2019,#2020,
#2021));
#2029=DERIVED_UNIT_ELEMENT(#2043,1.);
#2030=DERIVED_UNIT_ELEMENT(#9905,-3.);
#2031=DERIVED_UNIT_ELEMENT(#2043,1.);
#2032=DERIVED_UNIT_ELEMENT(#9905,-3.);
#2033=DERIVED_UNIT_ELEMENT(#2043,1.);
#2034=DERIVED_UNIT_ELEMENT(#9905,-3.);
#2035=DERIVED_UNIT_ELEMENT(#2043,1.);
#2036=DERIVED_UNIT_ELEMENT(#9905,-3.);
#2037=DERIVED_UNIT_ELEMENT(#2043,1.);
#2038=DERIVED_UNIT_ELEMENT(#9905,-3.);
#2039=DERIVED_UNIT_ELEMENT(#2043,1.);
#2040=DERIVED_UNIT_ELEMENT(#9905,-3.);
#2041=DERIVED_UNIT_ELEMENT(#2043,1.);
#2042=DERIVED_UNIT_ELEMENT(#9905,-3.);
#2043=(
MASS_UNIT()
NAMED_UNIT(*)
SI_UNIT(.KILO.,.GRAM.)
);
#2044=DERIVED_UNIT((#2029,#2030));
#2045=DERIVED_UNIT((#2031,#2032));
#2046=DERIVED_UNIT((#2033,#2034));
#2047=DERIVED_UNIT((#2035,#2036));
#2048=DERIVED_UNIT((#2037,#2038));
#2049=DERIVED_UNIT((#2039,#2040));
#2050=DERIVED_UNIT((#2041,#2042));
#2051=MEASURE_REPRESENTATION_ITEM('density measure',
POSITIVE_RATIO_MEASURE(7850.),#2044);
#2052=MEASURE_REPRESENTATION_ITEM('density measure',
POSITIVE_RATIO_MEASURE(7850.),#2045);
#2053=MEASURE_REPRESENTATION_ITEM('density measure',
POSITIVE_RATIO_MEASURE(7850.),#2046);
#2054=MEASURE_REPRESENTATION_ITEM('density measure',
POSITIVE_RATIO_MEASURE(7850.),#2047);
#2055=MEASURE_REPRESENTATION_ITEM('density measure',
POSITIVE_RATIO_MEASURE(7850.),#2048);
#2056=MEASURE_REPRESENTATION_ITEM('density measure',
POSITIVE_RATIO_MEASURE(7850.),#2049);
#2057=MEASURE_REPRESENTATION_ITEM('density measure',
POSITIVE_RATIO_MEASURE(7850.),#2050);
#2058=PROPERTY_DEFINITION_REPRESENTATION(#2093,#2072);
#2059=PROPERTY_DEFINITION_REPRESENTATION(#2094,#2073);
#2060=PROPERTY_DEFINITION_REPRESENTATION(#2095,#2074);
#2061=PROPERTY_DEFINITION_REPRESENTATION(#2096,#2075);
#2062=PROPERTY_DEFINITION_REPRESENTATION(#2097,#2076);
#2063=PROPERTY_DEFINITION_REPRESENTATION(#2098,#2077);
#2064=PROPERTY_DEFINITION_REPRESENTATION(#2099,#2078);
#2065=PROPERTY_DEFINITION_REPRESENTATION(#2100,#2079);
#2066=PROPERTY_DEFINITION_REPRESENTATION(#2101,#2080);
#2067=PROPERTY_DEFINITION_REPRESENTATION(#2102,#2081);
#2068=PROPERTY_DEFINITION_REPRESENTATION(#2103,#2082);
#2069=PROPERTY_DEFINITION_REPRESENTATION(#2104,#2083);
#2070=PROPERTY_DEFINITION_REPRESENTATION(#2105,#2084);
#2071=PROPERTY_DEFINITION_REPRESENTATION(#2106,#2085);
#2072=REPRESENTATION('material name',(#2086),#9896);
#2073=REPRESENTATION('density',(#2051),#9896);
#2074=REPRESENTATION('material name',(#2087),#9897);
#2075=REPRESENTATION('density',(#2052),#9897);
#2076=REPRESENTATION('material name',(#2088),#9898);
#2077=REPRESENTATION('density',(#2053),#9898);
#2078=REPRESENTATION('material name',(#2089),#9899);
#2079=REPRESENTATION('density',(#2054),#9899);
#2080=REPRESENTATION('material name',(#2090),#9900);
#2081=REPRESENTATION('density',(#2055),#9900);
#2082=REPRESENTATION('material name',(#2091),#9901);
#2083=REPRESENTATION('density',(#2056),#9901);
#2084=REPRESENTATION('material name',(#2092),#9902);
#2085=REPRESENTATION('density',(#2057),#9902);
#2086=DESCRIPTIVE_REPRESENTATION_ITEM('Steel','Steel');
#2087=DESCRIPTIVE_REPRESENTATION_ITEM('Steel','Steel');
#2088=DESCRIPTIVE_REPRESENTATION_ITEM('Steel','Steel');
#2089=DESCRIPTIVE_REPRESENTATION_ITEM('Steel','Steel');
#2090=DESCRIPTIVE_REPRESENTATION_ITEM('Steel','Steel');
#2091=DESCRIPTIVE_REPRESENTATION_ITEM('Steel','Steel');
#2092=DESCRIPTIVE_REPRESENTATION_ITEM('Steel','Steel');
#2093=PROPERTY_DEFINITION('material property','material name',#9947);
#2094=PROPERTY_DEFINITION('material property','density of part',#9947);
#2095=PROPERTY_DEFINITION('material property','material name',#9948);
#2096=PROPERTY_DEFINITION('material property','density of part',#9948);
#2097=PROPERTY_DEFINITION('material property','material name',#9949);
#2098=PROPERTY_DEFINITION('material property','density of part',#9949);
#2099=PROPERTY_DEFINITION('material property','material name',#9950);
#2100=PROPERTY_DEFINITION('material property','density of part',#9950);
#2101=PROPERTY_DEFINITION('material property','material name',#9951);
#2102=PROPERTY_DEFINITION('material property','density of part',#9951);
#2103=PROPERTY_DEFINITION('material property','material name',#9952);
#2104=PROPERTY_DEFINITION('material property','density of part',#9952);
#2105=PROPERTY_DEFINITION('material property','material name',#9953);
#2106=PROPERTY_DEFINITION('material property','density of part',#9953);
#2107=AXIS2_PLACEMENT_3D('',#2876,#2318,#2319);
#2108=AXIS2_PLACEMENT_3D('',#2877,#2320,#2321);
#2109=AXIS2_PLACEMENT_3D('',#2878,#2322,#2323);
#2110=AXIS2_PLACEMENT_3D('',#2880,#2324,#2325);
#2111=AXIS2_PLACEMENT_3D('',#2883,#2327,#2328);
#2112=AXIS2_PLACEMENT_3D('',#2884,#2329,#2330);
#2113=AXIS2_PLACEMENT_3D('',#2886,#2331,#2332);
#2114=AXIS2_PLACEMENT_3D('',#2889,#2334,#2335);
#2115=AXIS2_PLACEMENT_3D('',#2890,#2336,#2337);
#2116=AXIS2_PLACEMENT_3D('',#2891,#2338,#2339);
#2117=AXIS2_PLACEMENT_3D('',#2892,#2340,#2341);
#2118=AXIS2_PLACEMENT_3D('',#2893,#2342,#2343);
#2119=AXIS2_PLACEMENT_3D('',#2895,#2344,#2345);
#2120=AXIS2_PLACEMENT_3D('',#2897,#2346,#2347);
#2121=AXIS2_PLACEMENT_3D('',#2899,#2348,#2349);
#2122=AXIS2_PLACEMENT_3D('',#2900,#2350,#2351);
#2123=AXIS2_PLACEMENT_3D('',#2901,#2352,#2353);
#2124=AXIS2_PLACEMENT_3D('',#2904,#2354,#2355);
#2125=AXIS2_PLACEMENT_3D('',#2905,#2356,#2357);
#2126=AXIS2_PLACEMENT_3D('',#2907,#2358,#2359);
#2127=AXIS2_PLACEMENT_3D('',#2908,#2360,#2361);
#2128=AXIS2_PLACEMENT_3D('',#2909,#2362,#2363);
#2129=AXIS2_PLACEMENT_3D('',#2915,#2366,#2367);
#2130=AXIS2_PLACEMENT_3D('',#2918,#2369,#2370);
#2131=AXIS2_PLACEMENT_3D('',#2923,#2372,#2373);
#2132=AXIS2_PLACEMENT_3D('',#2926,#2375,#2376);
#2133=AXIS2_PLACEMENT_3D('',#2927,#2377,#2378);
#2134=AXIS2_PLACEMENT_3D('',#2928,#2379,#2380);
#2135=AXIS2_PLACEMENT_3D('',#2929,#2381,#2382);
#2136=AXIS2_PLACEMENT_3D('',#2932,#2385,#2386);
#2137=AXIS2_PLACEMENT_3D('',#2933,#2387,#2388);
#2138=AXIS2_PLACEMENT_3D('',#2934,#2389,#2390);
#2139=AXIS2_PLACEMENT_3D('',#2937,#2393,#2394);
#2140=AXIS2_PLACEMENT_3D('',#2938,#2395,#2396);
#2141=AXIS2_PLACEMENT_3D('',#2939,#2397,#2398);
#2142=AXIS2_PLACEMENT_3D('',#2940,#2399,#2400);
#2143=AXIS2_PLACEMENT_3D('',#2942,#2401,#2402);
#2144=AXIS2_PLACEMENT_3D('',#2944,#2403,#2404);
#2145=AXIS2_PLACEMENT_3D('',#2946,#2405,#2406);
#2146=AXIS2_PLACEMENT_3D('',#2947,#2407,#2408);
#2147=AXIS2_PLACEMENT_3D('',#2948,#2409,#2410);
#2148=AXIS2_PLACEMENT_3D('',#2950,#2411,#2412);
#2149=AXIS2_PLACEMENT_3D('',#2953,#2414,#2415);
#2150=AXIS2_PLACEMENT_3D('',#2954,#2416,#2417);
#2151=AXIS2_PLACEMENT_3D('',#2956,#2418,#2419);
#2152=AXIS2_PLACEMENT_3D('',#2958,#2420,#2421);
#2153=AXIS2_PLACEMENT_3D('',#2959,#2422,#2423);
#2154=AXIS2_PLACEMENT_3D('',#2960,#2424,#2425);
#2155=AXIS2_PLACEMENT_3D('',#2963,#2427,#2428);
#2156=AXIS2_PLACEMENT_3D('',#2964,#2429,#2430);
#2157=AXIS2_PLACEMENT_3D('',#2966,#2431,#2432);
#2158=AXIS2_PLACEMENT_3D('',#2969,#2434,#2435);
#2159=AXIS2_PLACEMENT_3D('',#2970,#2436,#2437);
#2160=AXIS2_PLACEMENT_3D('',#2972,#2438,#2439);
#2161=AXIS2_PLACEMENT_3D('',#2973,#2440,#2441);
#2162=AXIS2_PLACEMENT_3D('',#2974,#2442,#2443);
#2163=AXIS2_PLACEMENT_3D('',#2976,#2444,#2445);
#2164=AXIS2_PLACEMENT_3D('',#2978,#2446,#2447);
#2165=AXIS2_PLACEMENT_3D('',#2979,#2448,#2449);
#2166=AXIS2_PLACEMENT_3D('',#2980,#2450,#2451);
#2167=AXIS2_PLACEMENT_3D('',#2983,#2453,#2454);
#2168=AXIS2_PLACEMENT_3D('',#2984,#2455,#2456);
#2169=AXIS2_PLACEMENT_3D('',#2986,#2457,#2458);
#2170=AXIS2_PLACEMENT_3D('',#2989,#2460,#2461);
#2171=AXIS2_PLACEMENT_3D('',#2990,#2462,#2463);
#2172=AXIS2_PLACEMENT_3D('',#2992,#2465,#2466);
#2173=AXIS2_PLACEMENT_3D('',#2995,#2467,#2468);
#2174=AXIS2_PLACEMENT_3D('',#2997,#2470,#2471);
#2175=AXIS2_PLACEMENT_3D('',#2998,#2472,#2473);
#2176=AXIS2_PLACEMENT_3D('',#3001,#2475,#2476);
#2177=AXIS2_PLACEMENT_3D('',#3002,#2477,#2478);
#2178=AXIS2_PLACEMENT_3D('',#3004,#2479,#2480);
#2179=AXIS2_PLACEMENT_3D('',#3007,#2482,#2483);
#2180=AXIS2_PLACEMENT_3D('',#3008,#2484,#2485);
#2181=AXIS2_PLACEMENT_3D('',#3010,#2486,#2487);
#2182=AXIS2_PLACEMENT_3D('',#3011,#2488,#2489);
#2183=AXIS2_PLACEMENT_3D('',#3012,#2490,#2491);
#2184=AXIS2_PLACEMENT_3D('',#3013,#2492,#2493);
#2185=AXIS2_PLACEMENT_3D('',#3014,#2494,#2495);
#2186=AXIS2_PLACEMENT_3D('',#3015,#2496,#2497);
#2187=AXIS2_PLACEMENT_3D('',#3016,#2498,#2499);
#2188=AXIS2_PLACEMENT_3D('',#3017,#2500,#2501);
#2189=AXIS2_PLACEMENT_3D('',#3018,#2502,#2503);
#2190=AXIS2_PLACEMENT_3D('',#3019,#2504,#2505);
#2191=AXIS2_PLACEMENT_3D('',#3021,#2506,#2507);
#2192=AXIS2_PLACEMENT_3D('',#3024,#2509,#2510);
#2193=AXIS2_PLACEMENT_3D('',#3025,#2511,#2512);
#2194=AXIS2_PLACEMENT_3D('',#3027,#2513,#2514);
#2195=AXIS2_PLACEMENT_3D('',#3030,#2516,#2517);
#2196=AXIS2_PLACEMENT_3D('',#3031,#2518,#2519);
#2197=AXIS2_PLACEMENT_3D('',#3032,#2520,#2521);
#2198=AXIS2_PLACEMENT_3D('',#3033,#2522,#2523);
#2199=AXIS2_PLACEMENT_3D('',#3034,#2524,#2525);
#2200=AXIS2_PLACEMENT_3D('',#3036,#2526,#2527);
#2201=AXIS2_PLACEMENT_3D('',#3039,#2529,#2530);
#2202=AXIS2_PLACEMENT_3D('',#3040,#2531,#2532);
#2203=AXIS2_PLACEMENT_3D('',#3042,#2533,#2534);
#2204=AXIS2_PLACEMENT_3D('',#3045,#2536,#2537);
#2205=AXIS2_PLACEMENT_3D('',#3046,#2538,#2539);
#2206=AXIS2_PLACEMENT_3D('',#3048,#2540,#2541);
#2207=AXIS2_PLACEMENT_3D('',#3051,#2543,#2544);
#2208=AXIS2_PLACEMENT_3D('',#3052,#2545,#2546);
#2209=AXIS2_PLACEMENT_3D('',#3054,#2547,#2548);
#2210=AXIS2_PLACEMENT_3D('',#3057,#2550,#2551);
#2211=AXIS2_PLACEMENT_3D('',#3058,#2552,#2553);
#2212=AXIS2_PLACEMENT_3D('',#3067,#2558,#2559);
#2213=AXIS2_PLACEMENT_3D('',#3076,#2564,#2565);
#2214=AXIS2_PLACEMENT_3D('',#3087,#2572,#2573);
#2215=AXIS2_PLACEMENT_3D('',#3093,#2577,#2578);
#2216=AXIS2_PLACEMENT_3D('',#3101,#2584,#2585);
#2217=AXIS2_PLACEMENT_3D('',#3102,#2586,#2587);
#2218=AXIS2_PLACEMENT_3D('',#3104,#2589,#2590);
#2219=AXIS2_PLACEMENT_3D('',#3105,#2591,#2592);
#2220=AXIS2_PLACEMENT_3D('',#3107,#2594,#2595);
#2221=AXIS2_PLACEMENT_3D('',#3108,#2596,#2597);
#2222=AXIS2_PLACEMENT_3D('',#3109,#2598,#2599);
#2223=AXIS2_PLACEMENT_3D('',#3111,#2600,#2601);
#2224=AXIS2_PLACEMENT_3D('',#3114,#2603,#2604);
#2225=AXIS2_PLACEMENT_3D('',#3115,#2605,#2606);
#2226=AXIS2_PLACEMENT_3D('',#3117,#2607,#2608);
#2227=AXIS2_PLACEMENT_3D('',#3120,#2610,#2611);
#2228=AXIS2_PLACEMENT_3D('',#3121,#2612,#2613);
#2229=AXIS2_PLACEMENT_3D('',#3130,#2618,#2619);
#2230=AXIS2_PLACEMENT_3D('',#3139,#2624,#2625);
#2231=AXIS2_PLACEMENT_3D('',#3142,#2628,#2629);
#2232=AXIS2_PLACEMENT_3D('',#3144,#2631,#2632);
#2233=AXIS2_PLACEMENT_3D('',#3146,#2634,#2635);
#2234=AXIS2_PLACEMENT_3D('',#3147,#2636,#2637);
#2235=AXIS2_PLACEMENT_3D('',#3148,#2638,#2639);
#2236=AXIS2_PLACEMENT_3D('',#3165,#2641,#2642);
#2237=AXIS2_PLACEMENT_3D('',#3175,#2643,#2644);
#2238=AXIS2_PLACEMENT_3D('',#3205,#2646,#2647);
#2239=AXIS2_PLACEMENT_3D('',#3235,#2649,#2650);
#2240=AXIS2_PLACEMENT_3D('',#3265,#2652,#2653);
#2241=AXIS2_PLACEMENT_3D('',#3295,#2655,#2656);
#2242=AXIS2_PLACEMENT_3D('',#3325,#2658,#2659);
#2243=AXIS2_PLACEMENT_3D('',#3355,#2661,#2662);
#2244=AXIS2_PLACEMENT_3D('',#3385,#2664,#2665);
#2245=AXIS2_PLACEMENT_3D('',#3415,#2667,#2668);
#2246=AXIS2_PLACEMENT_3D('',#3445,#2670,#2671);
#2247=AXIS2_PLACEMENT_3D('',#3475,#2673,#2674);
#2248=AXIS2_PLACEMENT_3D('',#3505,#2676,#2677);
#2249=AXIS2_PLACEMENT_3D('',#3535,#2679,#2680);
#2250=AXIS2_PLACEMENT_3D('',#3561,#2682,#2683);
#2251=AXIS2_PLACEMENT_3D('',#3565,#2685,#2686);
#2252=AXIS2_PLACEMENT_3D('',#3566,#2687,#2688);
#2253=AXIS2_PLACEMENT_3D('',#3568,#2689,#2690);
#2254=AXIS2_PLACEMENT_3D('',#3585,#2691,#2692);
#2255=AXIS2_PLACEMENT_3D('',#3661,#2694,#2695);
#2256=AXIS2_PLACEMENT_3D('',#3737,#2697,#2698);
#2257=AXIS2_PLACEMENT_3D('',#3813,#2700,#2701);
#2258=AXIS2_PLACEMENT_3D('',#3889,#2703,#2704);
#2259=AXIS2_PLACEMENT_3D('',#3965,#2706,#2707);
#2260=AXIS2_PLACEMENT_3D('',#4043,#2709,#2710);
#2261=AXIS2_PLACEMENT_3D('',#4121,#2712,#2713);
#2262=AXIS2_PLACEMENT_3D('',#4197,#2715,#2716);
#2263=AXIS2_PLACEMENT_3D('',#4273,#2718,#2719);
#2264=AXIS2_PLACEMENT_3D('',#4349,#2721,#2722);
#2265=AXIS2_PLACEMENT_3D('',#4425,#2724,#2725);
#2266=AXIS2_PLACEMENT_3D('',#4501,#2727,#2728);
#2267=AXIS2_PLACEMENT_3D('',#4506,#2730,#2731);
#2268=AXIS2_PLACEMENT_3D('',#4557,#2732,#2733);
#2269=AXIS2_PLACEMENT_3D('',#4560,#2735,#2736);
#2270=AXIS2_PLACEMENT_3D('',#4562,#2737,#2738);
#2271=AXIS2_PLACEMENT_3D('',#4575,#2739,#2740);
#2272=AXIS2_PLACEMENT_3D('',#4577,#2741,#2742);
#2273=AXIS2_PLACEMENT_3D('',#4578,#2743,#2744);
#2274=AXIS2_PLACEMENT_3D('',#4579,#2745,#2746);
#2275=AXIS2_PLACEMENT_3D('',#4581,#2747,#2748);
#2276=AXIS2_PLACEMENT_3D('',#4583,#2749,#2750);
#2277=AXIS2_PLACEMENT_3D('',#4584,#2751,#2752);
#2278=AXIS2_PLACEMENT_3D('',#4585,#2753,#2754);
#2279=AXIS2_PLACEMENT_3D('',#4587,#2756,#2757);
#2280=AXIS2_PLACEMENT_3D('',#4593,#2758,#2759);
#2281=AXIS2_PLACEMENT_3D('',#4594,#2760,#2761);
#2282=AXIS2_PLACEMENT_3D('',#7215,#2762,#2763);
#2283=AXIS2_PLACEMENT_3D('',#9785,#2764,#2765);
#2284=AXIS2_PLACEMENT_3D('',#9786,#2766,#2767);
#2285=AXIS2_PLACEMENT_3D('',#9787,#2768,#2769);
#2286=AXIS2_PLACEMENT_3D('',#9800,#2776,#2777);
#2287=AXIS2_PLACEMENT_3D('',#9809,#2782,#2783);
#2288=AXIS2_PLACEMENT_3D('',#9815,#2787,#2788);
#2289=AXIS2_PLACEMENT_3D('',#9821,#2792,#2793);
#2290=AXIS2_PLACEMENT_3D('',#9827,#2797,#2798);
#2291=AXIS2_PLACEMENT_3D('',#9833,#2802,#2803);
#2292=AXIS2_PLACEMENT_3D('',#9836,#2806,#2807);
#2293=AXIS2_PLACEMENT_3D('',#9839,#2810,#2811);
#2294=AXIS2_PLACEMENT_3D('',#9841,#2813,#2814);
#2295=AXIS2_PLACEMENT_3D('',#9843,#2816,#2817);
#2296=AXIS2_PLACEMENT_3D('',#9845,#2819,#2820);
#2297=AXIS2_PLACEMENT_3D('',#9847,#2822,#2823);
#2298=AXIS2_PLACEMENT_3D('',#9848,#2824,#2825);
#2299=AXIS2_PLACEMENT_3D('',#9854,#2829,#2830);
#2300=AXIS2_PLACEMENT_3D('',#9858,#2833,#2834);
#2301=AXIS2_PLACEMENT_3D('',#9862,#2837,#2838);
#2302=AXIS2_PLACEMENT_3D('',#9866,#2841,#2842);
#2303=AXIS2_PLACEMENT_3D('',#9870,#2845,#2846);
#2304=AXIS2_PLACEMENT_3D('',#9872,#2848,#2849);
#2305=AXIS2_PLACEMENT_3D('',#9873,#2850,#2851);
#2306=AXIS2_PLACEMENT_3D('',#9874,#2852,#2853);
#2307=AXIS2_PLACEMENT_3D('',#9875,#2854,#2855);
#2308=AXIS2_PLACEMENT_3D('',#9876,#2856,#2857);
#2309=AXIS2_PLACEMENT_3D('',#9877,#2858,#2859);
#2310=AXIS2_PLACEMENT_3D('',#9878,#2860,#2861);
#2311=AXIS2_PLACEMENT_3D('',#9879,#2862,#2863);
#2312=AXIS2_PLACEMENT_3D('',#9880,#2864,#2865);
#2313=AXIS2_PLACEMENT_3D('',#9881,#2866,#2867);
#2314=AXIS2_PLACEMENT_3D('',#9882,#2868,#2869);
#2315=AXIS2_PLACEMENT_3D('',#9883,#2870,#2871);
#2316=AXIS2_PLACEMENT_3D('',#9884,#2872,#2873);
#2317=AXIS2_PLACEMENT_3D('',#9885,#2874,#2875);
#2318=DIRECTION('axis',(0.,0.,1.));
#2319=DIRECTION('refdir',(1.,0.,0.));
#2320=DIRECTION('axis',(0.,0.,1.));
#2321=DIRECTION('refdir',(1.,0.,0.));
#2322=DIRECTION('center_axis',(0.,0.,-1.));
#2323=DIRECTION('ref_axis',(-1.,0.,0.));
#2324=DIRECTION('center_axis',(0.,0.,1.));
#2325=DIRECTION('ref_axis',(1.,0.,0.));
#2326=DIRECTION('',(0.,0.,-1.));
#2327=DIRECTION('center_axis',(0.,0.,1.));
#2328=DIRECTION('ref_axis',(1.,0.,0.));
#2329=DIRECTION('center_axis',(0.,0.,-1.));
#2330=DIRECTION('ref_axis',(-1.,0.,0.));
#2331=DIRECTION('center_axis',(0.,0.,1.));
#2332=DIRECTION('ref_axis',(1.,0.,0.));
#2333=DIRECTION('',(0.,0.,1.));
#2334=DIRECTION('center_axis',(0.,0.,1.));
#2335=DIRECTION('ref_axis',(1.,0.,0.));
#2336=DIRECTION('center_axis',(0.,0.,1.));
#2337=DIRECTION('ref_axis',(1.,0.,0.));
#2338=DIRECTION('center_axis',(0.,0.,1.));
#2339=DIRECTION('ref_axis',(1.,0.,0.));
#2340=DIRECTION('axis',(0.,0.,1.));
#2341=DIRECTION('refdir',(1.,0.,0.));
#2342=DIRECTION('center_axis',(0.,0.,1.));
#2343=DIRECTION('ref_axis',(1.,0.,0.));
#2344=DIRECTION('center_axis',(0.,0.,1.));
#2345=DIRECTION('ref_axis',(1.,0.,0.));
#2346=DIRECTION('center_axis',(1.22464679914735E-16,-1.,0.));
#2347=DIRECTION('ref_axis',(-1.,-1.22464679914735E-16,0.));
#2348=DIRECTION('center_axis',(0.,0.,-1.));
#2349=DIRECTION('ref_axis',(1.,0.,0.));
#2350=DIRECTION('center_axis',(0.,0.,-1.));
#2351=DIRECTION('ref_axis',(1.,0.,0.));
#2352=DIRECTION('center_axis',(0.,0.,1.));
#2353=DIRECTION('ref_axis',(1.,0.,0.));
#2354=DIRECTION('center_axis',(0.,0.,1.));
#2355=DIRECTION('ref_axis',(1.,0.,0.));
#2356=DIRECTION('center_axis',(0.,0.,1.));
#2357=DIRECTION('ref_axis',(1.,0.,0.));
#2358=DIRECTION('center_axis',(1.22464679914735E-16,-1.,0.));
#2359=DIRECTION('ref_axis',(-1.,-1.22464679914735E-16,0.));
#2360=DIRECTION('center_axis',(0.,0.,-1.));
#2361=DIRECTION('ref_axis',(1.,0.,0.));
#2362=DIRECTION('center_axis',(0.,0.,-1.));
#2363=DIRECTION('ref_axis',(-1.,0.,0.));
#2364=DIRECTION('',(0.,0.,1.));
#2365=DIRECTION('',(0.,0.,1.));
#2366=DIRECTION('center_axis',(0.,0.,-1.));
#2367=DIRECTION('ref_axis',(-1.,0.,0.));
#2368=DIRECTION('',(0.,0.,-1.));
#2369=DIRECTION('center_axis',(0.,0.,-1.));
#2370=DIRECTION('ref_axis',(-1.,0.,0.));
#2371=DIRECTION('',(0.,0.,-1.));
#2372=DIRECTION('center_axis',(0.,0.,1.));
#2373=DIRECTION('ref_axis',(1.,0.,0.));
#2374=DIRECTION('',(0.,0.,1.));
#2375=DIRECTION('center_axis',(0.,0.,1.));
#2376=DIRECTION('ref_axis',(1.,0.,0.));
#2377=DIRECTION('center_axis',(0.,0.,1.));
#2378=DIRECTION('ref_axis',(1.,0.,0.));
#2379=DIRECTION('center_axis',(0.,0.,1.));
#2380=DIRECTION('ref_axis',(1.,0.,0.));
#2381=DIRECTION('center_axis',(0.,1.,0.));
#2382=DIRECTION('ref_axis',(0.,0.,1.));
#2383=DIRECTION('',(1.,0.,0.));
#2384=DIRECTION('',(1.,0.,0.));
#2385=DIRECTION('center_axis',(0.,0.,1.));
#2386=DIRECTION('ref_axis',(1.,0.,0.));
#2387=DIRECTION('center_axis',(0.,0.,1.));
#2388=DIRECTION('ref_axis',(1.,0.,0.));
#2389=DIRECTION('center_axis',(0.,1.,0.));
#2390=DIRECTION('ref_axis',(0.,0.,1.));
#2391=DIRECTION('',(-1.,0.,0.));
#2392=DIRECTION('',(-1.,0.,0.));
#2393=DIRECTION('center_axis',(0.,0.,-1.));
#2394=DIRECTION('ref_axis',(-1.,0.,0.));
#2395=DIRECTION('center_axis',(0.,0.,-1.));
#2396=DIRECTION('ref_axis',(-1.,0.,0.));
#2397=DIRECTION('axis',(0.,0.,1.));
#2398=DIRECTION('refdir',(1.,0.,0.));
#2399=DIRECTION('center_axis',(-1.,0.,0.));
#2400=DIRECTION('ref_axis',(0.,0.,1.));
#2401=DIRECTION('center_axis',(-1.,0.,0.));
#2402=DIRECTION('ref_axis',(0.,0.,1.));
#2403=DIRECTION('center_axis',(0.,1.,-1.22464679914735E-16));
#2404=DIRECTION('ref_axis',(0.,-1.22464679914735E-16,-1.));
#2405=DIRECTION('center_axis',(-1.,0.,0.));
#2406=DIRECTION('ref_axis',(0.,0.,1.));
#2407=DIRECTION('center_axis',(-1.,0.,0.));
#2408=DIRECTION('ref_axis',(0.,0.,1.));
#2409=DIRECTION('center_axis',(-1.,0.,0.));
#2410=DIRECTION('ref_axis',(0.,0.,1.));
#2411=DIRECTION('center_axis',(1.,0.,0.));
#2412=DIRECTION('ref_axis',(0.,0.,1.));
#2413=DIRECTION('',(-1.,0.,0.));
#2414=DIRECTION('center_axis',(-1.,0.,0.));
#2415=DIRECTION('ref_axis',(0.,0.,-1.));
#2416=DIRECTION('center_axis',(-1.,0.,0.));
#2417=DIRECTION('ref_axis',(0.,0.,1.));
#2418=DIRECTION('center_axis',(-1.,0.,0.));
#2419=DIRECTION('ref_axis',(0.,0.,1.));
#2420=DIRECTION('center_axis',(0.,1.,-1.22464679914735E-16));
#2421=DIRECTION('ref_axis',(0.,-1.22464679914735E-16,-1.));
#2422=DIRECTION('center_axis',(-1.,0.,0.));
#2423=DIRECTION('ref_axis',(0.,0.,1.));
#2424=DIRECTION('center_axis',(-1.,0.,0.));
#2425=DIRECTION('ref_axis',(0.,0.,1.));
#2426=DIRECTION('',(1.,0.,0.));
#2427=DIRECTION('center_axis',(-1.,0.,0.));
#2428=DIRECTION('ref_axis',(0.,0.,1.));
#2429=DIRECTION('center_axis',(-1.,0.,0.));
#2430=DIRECTION('ref_axis',(0.,0.,1.));
#2431=DIRECTION('center_axis',(-1.,0.,0.));
#2432=DIRECTION('ref_axis',(0.,0.,1.));
#2433=DIRECTION('',(1.,0.,0.));
#2434=DIRECTION('center_axis',(-1.,0.,0.));
#2435=DIRECTION('ref_axis',(0.,0.,1.));
#2436=DIRECTION('center_axis',(-1.,0.,0.));
#2437=DIRECTION('ref_axis',(0.,0.,1.));
#2438=DIRECTION('center_axis',(0.,1.,-1.22464679914735E-16));
#2439=DIRECTION('ref_axis',(0.,-1.22464679914735E-16,-1.));
#2440=DIRECTION('center_axis',(-1.,0.,0.));
#2441=DIRECTION('ref_axis',(0.,0.,1.));
#2442=DIRECTION('center_axis',(-1.,0.,0.));
#2443=DIRECTION('ref_axis',(0.,0.,1.));
#2444=DIRECTION('center_axis',(-1.,0.,0.));
#2445=DIRECTION('ref_axis',(0.,0.,1.));
#2446=DIRECTION('center_axis',(0.,1.,-1.22464679914735E-16));
#2447=DIRECTION('ref_axis',(0.,-1.22464679914735E-16,-1.));
#2448=DIRECTION('center_axis',(-1.,0.,0.));
#2449=DIRECTION('ref_axis',(0.,0.,1.));
#2450=DIRECTION('center_axis',(-1.,0.,0.));
#2451=DIRECTION('ref_axis',(0.,0.,1.));
#2452=DIRECTION('',(-1.,0.,0.));
#2453=DIRECTION('center_axis',(-1.,0.,0.));
#2454=DIRECTION('ref_axis',(0.,0.,1.));
#2455=DIRECTION('center_axis',(-1.,0.,0.));
#2456=DIRECTION('ref_axis',(0.,0.,1.));
#2457=DIRECTION('center_axis',(-1.,0.,0.));
#2458=DIRECTION('ref_axis',(0.,0.,1.));
#2459=DIRECTION('',(1.,0.,0.));
#2460=DIRECTION('center_axis',(-1.,0.,0.));
#2461=DIRECTION('ref_axis',(0.,0.,1.));
#2462=DIRECTION('center_axis',(-1.,0.,0.));
#2463=DIRECTION('ref_axis',(0.,0.,1.));
#2464=DIRECTION('',(0.358367949545298,1.14330628105642E-16,0.933580426497203));
#2465=DIRECTION('center_axis',(1.,0.,0.));
#2466=DIRECTION('ref_axis',(0.,0.,-1.));
#2467=DIRECTION('center_axis',(-1.,0.,0.));
#2468=DIRECTION('ref_axis',(0.,0.,1.));
#2469=DIRECTION('',(-0.358367949545298,1.14330628105642E-16,-0.933580426497203));
#2470=DIRECTION('center_axis',(-1.,0.,0.));
#2471=DIRECTION('ref_axis',(0.,0.,1.));
#2472=DIRECTION('center_axis',(-1.,0.,0.));
#2473=DIRECTION('ref_axis',(0.,0.,1.));
#2474=DIRECTION('',(1.,0.,0.));
#2475=DIRECTION('center_axis',(-1.,0.,0.));
#2476=DIRECTION('ref_axis',(0.,0.,1.));
#2477=DIRECTION('center_axis',(-1.,0.,0.));
#2478=DIRECTION('ref_axis',(0.,0.,1.));
#2479=DIRECTION('center_axis',(-1.,0.,0.));
#2480=DIRECTION('ref_axis',(0.,0.,1.));
#2481=DIRECTION('',(-1.,0.,0.));
#2482=DIRECTION('center_axis',(-1.,0.,0.));
#2483=DIRECTION('ref_axis',(0.,0.,1.));
#2484=DIRECTION('center_axis',(-1.,0.,0.));
#2485=DIRECTION('ref_axis',(0.,0.,1.));
#2486=DIRECTION('center_axis',(0.,1.,-1.22464679914735E-16));
#2487=DIRECTION('ref_axis',(0.,-1.22464679914735E-16,-1.));
#2488=DIRECTION('center_axis',(-1.,0.,0.));
#2489=DIRECTION('ref_axis',(0.,0.,1.));
#2490=DIRECTION('center_axis',(1.,0.,0.));
#2491=DIRECTION('ref_axis',(0.,0.,-1.));
#2492=DIRECTION('center_axis',(-1.,0.,0.));
#2493=DIRECTION('ref_axis',(0.,0.,1.));
#2494=DIRECTION('center_axis',(1.,0.,0.));
#2495=DIRECTION('ref_axis',(0.,0.,-1.));
#2496=DIRECTION('center_axis',(1.,0.,0.));
#2497=DIRECTION('ref_axis',(0.,0.,-1.));
#2498=DIRECTION('center_axis',(1.,0.,0.));
#2499=DIRECTION('ref_axis',(0.,0.,-1.));
#2500=DIRECTION('center_axis',(1.,0.,0.));
#2501=DIRECTION('ref_axis',(0.,0.,-1.));
#2502=DIRECTION('axis',(0.,0.,1.));
#2503=DIRECTION('refdir',(1.,0.,0.));
#2504=DIRECTION('center_axis',(-1.,0.,0.));
#2505=DIRECTION('ref_axis',(0.,0.,1.));
#2506=DIRECTION('center_axis',(-1.,0.,0.));
#2507=DIRECTION('ref_axis',(0.,0.,1.));
#2508=DIRECTION('',(-1.,0.,0.));
#2509=DIRECTION('center_axis',(-1.,0.,0.));
#2510=DIRECTION('ref_axis',(0.,0.,1.));
#2511=DIRECTION('center_axis',(-1.,0.,0.));
#2512=DIRECTION('ref_axis',(0.,0.,1.));
#2513=DIRECTION('center_axis',(-1.,0.,0.));
#2514=DIRECTION('ref_axis',(0.,0.,1.));
#2515=DIRECTION('',(1.,0.,0.));
#2516=DIRECTION('center_axis',(-1.,0.,0.));
#2517=DIRECTION('ref_axis',(0.,0.,1.));
#2518=DIRECTION('center_axis',(1.,0.,0.));
#2519=DIRECTION('ref_axis',(0.,0.,-1.));
#2520=DIRECTION('center_axis',(1.,0.,0.));
#2521=DIRECTION('ref_axis',(0.,0.,-1.));
#2522=DIRECTION('axis',(0.,0.,1.));
#2523=DIRECTION('refdir',(1.,0.,0.));
#2524=DIRECTION('center_axis',(0.,-1.,0.));
#2525=DIRECTION('ref_axis',(0.,0.,-1.));
#2526=DIRECTION('center_axis',(0.,-1.,0.));
#2527=DIRECTION('ref_axis',(0.,0.,-1.));
#2528=DIRECTION('',(0.,-1.,0.));
#2529=DIRECTION('center_axis',(0.,-1.,0.));
#2530=DIRECTION('ref_axis',(0.,0.,-1.));
#2531=DIRECTION('center_axis',(0.,0.,-1.));
#2532=DIRECTION('ref_axis',(-1.,0.,0.));
#2533=DIRECTION('center_axis',(0.,0.,1.));
#2534=DIRECTION('ref_axis',(1.,0.,0.));
#2535=DIRECTION('',(0.,0.,-1.));
#2536=DIRECTION('center_axis',(0.,0.,-1.));
#2537=DIRECTION('ref_axis',(-1.,0.,0.));
#2538=DIRECTION('center_axis',(0.,0.,-1.));
#2539=DIRECTION('ref_axis',(-1.,0.,0.));
#2540=DIRECTION('center_axis',(0.,0.,1.));
#2541=DIRECTION('ref_axis',(1.,0.,0.));
#2542=DIRECTION('',(0.,0.,-1.));
#2543=DIRECTION('center_axis',(0.,0.,-1.));
#2544=DIRECTION('ref_axis',(-1.,0.,0.));
#2545=DIRECTION('center_axis',(0.,0.,-1.));
#2546=DIRECTION('ref_axis',(-1.,0.,0.));
#2547=DIRECTION('center_axis',(0.,0.,1.));
#2548=DIRECTION('ref_axis',(1.,0.,0.));
#2549=DIRECTION('',(0.,0.,-1.));
#2550=DIRECTION('center_axis',(0.,0.,-1.));
#2551=DIRECTION('ref_axis',(-1.,0.,0.));
#2552=DIRECTION('center_axis',(0.,0.,1.));
#2553=DIRECTION('ref_axis',(1.,0.,0.));
#2554=DIRECTION('',(0.,-1.,0.));
#2555=DIRECTION('',(-1.,0.,0.));
#2556=DIRECTION('',(0.,1.,0.));
#2557=DIRECTION('',(1.,0.,0.));
#2558=DIRECTION('center_axis',(0.,1.,0.));
#2559=DIRECTION('ref_axis',(0.,0.,1.));
#2560=DIRECTION('',(1.,0.,0.));
#2561=DIRECTION('',(0.,0.,-1.));
#2562=DIRECTION('',(1.,0.,0.));
#2563=DIRECTION('',(0.,0.,-1.));
#2564=DIRECTION('center_axis',(-1.,0.,0.));
#2565=DIRECTION('ref_axis',(0.,0.,1.));
#2566=DIRECTION('',(0.,1.,0.));
#2567=DIRECTION('',(0.,0.,-1.));
#2568=DIRECTION('',(0.,1.,0.));
#2569=DIRECTION('',(0.,0.,-1.));
#2570=DIRECTION('',(0.,0.,-1.));
#2571=DIRECTION('',(0.,1.,0.));
#2572=DIRECTION('center_axis',(8.67361737988404E-17,-1.,0.));
#2573=DIRECTION('ref_axis',(1.,8.67361737988404E-17,0.));
#2574=DIRECTION('',(-1.,-8.67361737988404E-17,0.));
#2575=DIRECTION('',(0.,0.,-1.));
#2576=DIRECTION('',(-1.,-8.67361737988404E-17,0.));
#2577=DIRECTION('center_axis',(1.,0.,0.));
#2578=DIRECTION('ref_axis',(0.,0.,-1.));
#2579=DIRECTION('',(0.,-1.,0.));
#2580=DIRECTION('',(0.,-1.,0.));
#2581=DIRECTION('',(0.,0.,-1.));
#2582=DIRECTION('',(0.,0.,-1.));
#2583=DIRECTION('',(0.,-1.,0.));
#2584=DIRECTION('center_axis',(0.,0.,1.));
#2585=DIRECTION('ref_axis',(1.,0.,0.));
#2586=DIRECTION('center_axis',(0.,1.,0.));
#2587=DIRECTION('ref_axis',(0.,0.,1.));
#2588=DIRECTION('',(1.,0.,0.));
#2589=DIRECTION('center_axis',(0.,0.,1.));
#2590=DIRECTION('ref_axis',(1.,0.,0.));
#2591=DIRECTION('center_axis',(0.,-1.,0.));
#2592=DIRECTION('ref_axis',(0.,0.,-1.));
#2593=DIRECTION('',(-1.,0.,0.));
#2594=DIRECTION('center_axis',(0.,0.,-1.));
#2595=DIRECTION('ref_axis',(-1.,0.,0.));
#2596=DIRECTION('axis',(0.,0.,1.));
#2597=DIRECTION('refdir',(1.,0.,0.));
#2598=DIRECTION('center_axis',(0.,0.,-1.));
#2599=DIRECTION('ref_axis',(-1.,0.,0.));
#2600=DIRECTION('center_axis',(0.,0.,1.));
#2601=DIRECTION('ref_axis',(1.,0.,0.));
#2602=DIRECTION('',(0.,0.,-1.));
#2603=DIRECTION('center_axis',(0.,0.,1.));
#2604=DIRECTION('ref_axis',(1.,0.,0.));
#2605=DIRECTION('center_axis',(0.,0.,-1.));
#2606=DIRECTION('ref_axis',(-1.,0.,0.));
#2607=DIRECTION('center_axis',(0.,0.,1.));
#2608=DIRECTION('ref_axis',(1.,0.,0.));
#2609=DIRECTION('',(0.,0.,-1.));
#2610=DIRECTION('center_axis',(0.,0.,1.));
#2611=DIRECTION('ref_axis',(1.,0.,0.));
#2612=DIRECTION('center_axis',(0.,0.,1.));
#2613=DIRECTION('ref_axis',(1.,0.,0.));
#2614=DIRECTION('',(0.,-1.,0.));
#2615=DIRECTION('',(1.,0.,0.));
#2616=DIRECTION('',(0.,1.,0.));
#2617=DIRECTION('',(-1.,0.,0.));
#2618=DIRECTION('center_axis',(0.,0.,1.));
#2619=DIRECTION('ref_axis',(1.,0.,0.));
#2620=DIRECTION('',(0.,-1.,0.));
#2621=DIRECTION('',(-1.,0.,0.));
#2622=DIRECTION('',(0.,1.,0.));
#2623=DIRECTION('',(1.,0.,0.));
#2624=DIRECTION('center_axis',(1.,0.,0.));
#2625=DIRECTION('ref_axis',(0.,0.,-1.));
#2626=DIRECTION('',(0.,0.,-1.));
#2627=DIRECTION('',(0.,0.,-1.));
#2628=DIRECTION('center_axis',(0.,1.,0.));
#2629=DIRECTION('ref_axis',(0.,0.,1.));
#2630=DIRECTION('',(0.,0.,-1.));
#2631=DIRECTION('center_axis',(-1.,0.,0.));
#2632=DIRECTION('ref_axis',(0.,0.,1.));
#2633=DIRECTION('',(0.,0.,-1.));
#2634=DIRECTION('center_axis',(0.,-1.,0.));
#2635=DIRECTION('ref_axis',(0.,0.,-1.));
#2636=DIRECTION('axis',(0.,0.,1.));
#2637=DIRECTION('refdir',(1.,0.,0.));
#2638=DIRECTION('center_axis',(0.,-1.,0.));
#2639=DIRECTION('ref_axis',(-1.,0.,1.28409742660487E-16));
#2640=DIRECTION('',(0.,1.,0.));
#2641=DIRECTION('center_axis',(0.,-1.,0.));
#2642=DIRECTION('ref_axis',(-1.,0.,1.28409742660487E-16));
#2643=DIRECTION('center_axis',(0.,-1.,0.));
#2644=DIRECTION('ref_axis',(-1.,0.,1.28409742660487E-16));
#2645=DIRECTION('',(0.,1.,0.));
#2646=DIRECTION('center_axis',(0.,-1.,0.));
#2647=DIRECTION('ref_axis',(-1.,0.,1.28409742660487E-16));
#2648=DIRECTION('',(0.,1.,0.));
#2649=DIRECTION('center_axis',(0.,-1.,0.));
#2650=DIRECTION('ref_axis',(-1.,0.,1.28409742660487E-16));
#2651=DIRECTION('',(0.,1.,0.));
#2652=DIRECTION('center_axis',(0.,-1.,0.));
#2653=DIRECTION('ref_axis',(-1.,0.,1.28409742660487E-16));
#2654=DIRECTION('',(0.,1.,0.));
#2655=DIRECTION('center_axis',(0.,-1.,0.));
#2656=DIRECTION('ref_axis',(-1.,0.,1.28409742660487E-16));
#2657=DIRECTION('',(0.,1.,0.));
#2658=DIRECTION('center_axis',(0.,-1.,0.));
#2659=DIRECTION('ref_axis',(-1.,0.,1.28409742660487E-16));
#2660=DIRECTION('',(0.,1.,0.));
#2661=DIRECTION('center_axis',(0.,-1.,0.));
#2662=DIRECTION('ref_axis',(-1.,0.,1.28409742660487E-16));
#2663=DIRECTION('',(0.,1.,0.));
#2664=DIRECTION('center_axis',(0.,-1.,0.));
#2665=DIRECTION('ref_axis',(-1.,0.,1.28409742660487E-16));
#2666=DIRECTION('',(0.,1.,0.));
#2667=DIRECTION('center_axis',(0.,-1.,0.));
#2668=DIRECTION('ref_axis',(-1.,0.,1.28409742660487E-16));
#2669=DIRECTION('',(0.,1.,0.));
#2670=DIRECTION('center_axis',(0.,-1.,0.));
#2671=DIRECTION('ref_axis',(-1.,0.,1.28409742660487E-16));
#2672=DIRECTION('',(0.,1.,0.));
#2673=DIRECTION('center_axis',(0.,-1.,0.));
#2674=DIRECTION('ref_axis',(-1.,0.,1.28409742660487E-16));
#2675=DIRECTION('',(0.,1.,0.));
#2676=DIRECTION('center_axis',(0.,-1.,0.));
#2677=DIRECTION('ref_axis',(-1.,0.,1.28409742660487E-16));
#2678=DIRECTION('',(0.,1.,0.));
#2679=DIRECTION('center_axis',(0.,-1.,0.));
#2680=DIRECTION('ref_axis',(0.,0.,-1.));
#2681=DIRECTION('',(0.,1.,0.));
#2682=DIRECTION('center_axis',(0.,1.,0.));
#2683=DIRECTION('ref_axis',(0.,0.,1.));
#2684=DIRECTION('',(0.,1.,0.));
#2685=DIRECTION('center_axis',(0.,-1.,0.));
#2686=DIRECTION('ref_axis',(0.,0.,1.));
#2687=DIRECTION('center_axis',(0.,-1.,0.));
#2688=DIRECTION('ref_axis',(0.,0.,1.));
#2689=DIRECTION('center_axis',(0.,1.,0.));
#2690=DIRECTION('ref_axis',(0.,0.,1.));
#2691=DIRECTION('center_axis',(0.,-1.,0.));
#2692=DIRECTION('ref_axis',(0.,0.,-1.));
#2693=DIRECTION('',(0.,1.,0.));
#2694=DIRECTION('center_axis',(0.,-1.,0.));
#2695=DIRECTION('ref_axis',(0.,0.,-1.));
#2696=DIRECTION('',(0.,1.,0.));
#2697=DIRECTION('center_axis',(0.,-1.,0.));
#2698=DIRECTION('ref_axis',(0.,0.,-1.));
#2699=DIRECTION('',(0.,1.,0.));
#2700=DIRECTION('center_axis',(0.,-1.,0.));
#2701=DIRECTION('ref_axis',(0.,0.,-1.));
#2702=DIRECTION('',(0.,1.,0.));
#2703=DIRECTION('center_axis',(0.,-1.,0.));
#2704=DIRECTION('ref_axis',(0.,0.,-1.));
#2705=DIRECTION('',(0.,1.,0.));
#2706=DIRECTION('center_axis',(0.,-1.,0.));
#2707=DIRECTION('ref_axis',(0.,0.,-1.));
#2708=DIRECTION('',(0.,1.,0.));
#2709=DIRECTION('center_axis',(0.,-1.,0.));
#2710=DIRECTION('ref_axis',(0.,0.,-1.));
#2711=DIRECTION('',(0.,1.,0.));
#2712=DIRECTION('center_axis',(0.,-1.,0.));
#2713=DIRECTION('ref_axis',(0.,0.,-1.));
#2714=DIRECTION('',(0.,1.,0.));
#2715=DIRECTION('center_axis',(0.,-1.,0.));
#2716=DIRECTION('ref_axis',(0.,0.,-1.));
#2717=DIRECTION('',(0.,1.,0.));
#2718=DIRECTION('center_axis',(0.,-1.,0.));
#2719=DIRECTION('ref_axis',(0.,0.,-1.));
#2720=DIRECTION('',(0.,1.,0.));
#2721=DIRECTION('center_axis',(0.,-1.,0.));
#2722=DIRECTION('ref_axis',(0.,0.,-1.));
#2723=DIRECTION('',(0.,1.,0.));
#2724=DIRECTION('center_axis',(0.,-1.,0.));
#2725=DIRECTION('ref_axis',(0.,0.,-1.));
#2726=DIRECTION('',(0.,1.,0.));
#2727=DIRECTION('center_axis',(0.,1.,0.));
#2728=DIRECTION('ref_axis',(0.,0.,1.));
#2729=DIRECTION('',(8.65956056235498E-17,-0.707106781186544,0.707106781186551));
#2730=DIRECTION('center_axis',(0.,1.,0.));
#2731=DIRECTION('ref_axis',(0.,0.,1.));
#2732=DIRECTION('center_axis',(-8.64437306947178E-16,-1.,-1.44797790076548E-15));
#2733=DIRECTION('ref_axis',(0.961856708765554,-4.33382881479145E-16,-0.273553782285489));
#2734=DIRECTION('',(8.65956056235498E-17,-0.707106781186544,0.707106781186551));
#2735=DIRECTION('center_axis',(0.,-1.,0.));
#2736=DIRECTION('ref_axis',(0.,0.,-1.));
#2737=DIRECTION('center_axis',(-8.64437306947178E-16,-1.,-1.44797790076548E-15));
#2738=DIRECTION('ref_axis',(0.961856708765554,-4.33382881479145E-16,-0.273553782285489));
#2739=DIRECTION('center_axis',(0.,1.,0.));
#2740=DIRECTION('ref_axis',(0.,0.,1.));
#2741=DIRECTION('center_axis',(0.,1.,0.));
#2742=DIRECTION('ref_axis',(0.,0.,1.));
#2743=DIRECTION('center_axis',(1.,0.,-1.22464679914735E-16));
#2744=DIRECTION('ref_axis',(-1.22464679914735E-16,0.,-1.));
#2745=DIRECTION('center_axis',(0.,1.,0.));
#2746=DIRECTION('ref_axis',(0.,0.,1.));
#2747=DIRECTION('center_axis',(0.,1.,0.));
#2748=DIRECTION('ref_axis',(0.,0.,1.));
#2749=DIRECTION('center_axis',(-1.,0.,1.22464679914735E-16));
#2750=DIRECTION('ref_axis',(-1.22464679914735E-16,0.,-1.));
#2751=DIRECTION('center_axis',(0.,-1.,0.));
#2752=DIRECTION('ref_axis',(0.,0.,1.));
#2753=DIRECTION('center_axis',(0.,1.,0.));
#2754=DIRECTION('ref_axis',(0.,0.,1.));
#2755=DIRECTION('',(8.65956056235495E-17,-0.707106781186546,0.707106781186549));
#2756=DIRECTION('center_axis',(0.,1.,0.));
#2757=DIRECTION('ref_axis',(0.,0.,1.));
#2758=DIRECTION('center_axis',(0.,1.,0.));
#2759=DIRECTION('ref_axis',(0.,0.,1.));
#2760=DIRECTION('center_axis',(0.,-1.,0.));
#2761=DIRECTION('ref_axis',(0.,0.,-1.));
#2762=DIRECTION('center_axis',(0.,-1.,0.));
#2763=DIRECTION('ref_axis',(-1.,0.,1.28409742660487E-16));
#2764=DIRECTION('center_axis',(0.,1.,0.));
#2765=DIRECTION('ref_axis',(0.,0.,1.));
#2766=DIRECTION('center_axis',(0.,1.,0.));
#2767=DIRECTION('ref_axis',(0.,0.,1.));
#2768=DIRECTION('center_axis',(0.,1.,0.));
#2769=DIRECTION('ref_axis',(0.,0.,1.));
#2770=DIRECTION('',(-0.866025403784438,0.,-0.5));
#2771=DIRECTION('',(0.,0.,-1.));
#2772=DIRECTION('',(0.866025403784439,0.,-0.5));
#2773=DIRECTION('',(0.866025403784438,0.,0.5));
#2774=DIRECTION('',(1.50231459873716E-16,0.,1.));
#2775=DIRECTION('',(-0.866025403784439,0.,0.5));
#2776=DIRECTION('center_axis',(0.5,0.,-0.866025403784439));
#2777=DIRECTION('ref_axis',(-0.866025403784439,0.,-0.5));
#2778=DIRECTION('',(0.,1.,0.));
#2779=DIRECTION('',(-0.866025403784439,0.,-0.5));
#2780=DIRECTION('',(0.,1.,0.));
#2781=DIRECTION('',(-0.866025403784439,0.,-0.5));
#2782=DIRECTION('center_axis',(1.,0.,-1.50231459873716E-16));
#2783=DIRECTION('ref_axis',(-1.50231459873716E-16,0.,-1.));
#2784=DIRECTION('',(0.,1.,0.));
#2785=DIRECTION('',(-1.50231459873716E-16,0.,-1.));
#2786=DIRECTION('',(-1.50231459873716E-16,0.,-1.));
#2787=DIRECTION('center_axis',(0.5,0.,0.866025403784439));
#2788=DIRECTION('ref_axis',(0.866025403784439,0.,-0.5));
#2789=DIRECTION('',(0.,1.,0.));
#2790=DIRECTION('',(0.866025403784439,0.,-0.5));
#2791=DIRECTION('',(0.866025403784439,0.,-0.5));
#2792=DIRECTION('center_axis',(-0.5,0.,0.866025403784439));
#2793=DIRECTION('ref_axis',(0.866025403784439,0.,0.5));
#2794=DIRECTION('',(0.,1.,0.));
#2795=DIRECTION('',(0.866025403784438,0.,0.5));
#2796=DIRECTION('',(0.866025403784438,0.,0.5));
#2797=DIRECTION('center_axis',(-1.,0.,0.));
#2798=DIRECTION('ref_axis',(0.,0.,1.));
#2799=DIRECTION('',(0.,1.,0.));
#2800=DIRECTION('',(0.,0.,1.));
#2801=DIRECTION('',(0.,0.,1.));
#2802=DIRECTION('center_axis',(-0.5,0.,-0.866025403784439));
#2803=DIRECTION('ref_axis',(-0.866025403784439,0.,0.5));
#2804=DIRECTION('',(-0.866025403784439,0.,0.5));
#2805=DIRECTION('',(-0.866025403784439,0.,0.5));
#2806=DIRECTION('center_axis',(-0.70710678118655,0.707106781186545,1.0622968402426E-16));
#2807=DIRECTION('ref_axis',(1.50231459873716E-16,2.12845086949137E-34,1.));
#2808=DIRECTION('',(-0.654653670707975,-0.65465367070798,-0.377964473009225));
#2809=DIRECTION('',(0.654653670707975,0.65465367070798,-0.377964473009227));
#2810=DIRECTION('center_axis',(-0.353553390593275,0.707106781186545,0.612372435695797));
#2811=DIRECTION('ref_axis',(0.866025403784439,1.12179404366126E-17,0.5));
#2812=DIRECTION('',(4.73877874074079E-16,0.65465367070798,-0.755928946018452));
#2813=DIRECTION('center_axis',(-0.353553390593275,0.707106781186544,-0.612372435695797));
#2814=DIRECTION('ref_axis',(-0.866025403784439,-2.22179676214442E-17,0.5));
#2815=DIRECTION('',(2.46349614890202E-15,-0.65465367070798,-0.755928946018452));
#2816=DIRECTION('center_axis',(0.353553390593275,0.707106781186545,0.612372435695797));
#2817=DIRECTION('ref_axis',(0.866025403784439,6.5167186869869E-18,-0.5));
#2818=DIRECTION('',(-0.654653670707975,0.65465367070798,-0.377964473009226));
#2819=DIRECTION('center_axis',(0.353553390593275,0.707106781186546,-0.612372435695796));
#2820=DIRECTION('ref_axis',(-0.866025403784439,3.51850444550808E-18,-0.5));
#2821=DIRECTION('',(0.654653670707975,-0.654653670707979,-0.377964473009227));
#2822=DIRECTION('center_axis',(0.70710678118655,0.707106781186545,0.));
#2823=DIRECTION('ref_axis',(0.,0.,-1.));
#2824=DIRECTION('center_axis',(0.249999999999997,-0.86602540378444,-0.433012701892219));
#2825=DIRECTION('ref_axis',(1.15617626223753E-17,0.447213595499957,-0.894427190999916));
#2826=DIRECTION('',(-3.0099126994645E-15,0.447213595499957,-0.894427190999917));
#2827=DIRECTION('',(-0.866025403784441,0.,-0.499999999999995));
#2828=DIRECTION('',(0.77459666924148,0.447213595499957,-0.447213595499965));
#2829=DIRECTION('center_axis',(0.499999999999998,-0.86602540378444,-5.25810109558002E-15));
#2830=DIRECTION('ref_axis',(0.86602540378444,0.499999999999998,-1.39303110180435E-31));
#2831=DIRECTION('',(-1.05162021911601E-14,0.,-1.));
#2832=DIRECTION('',(0.774596669241488,0.447213595499956,0.447213595499951));
#2833=DIRECTION('center_axis',(0.250000000000003,-0.86602540378444,0.433012701892216));
#2834=DIRECTION('ref_axis',(-1.269494574772E-17,-0.447213595499954,-0.894427190999918));
#2835=DIRECTION('',(0.866025403784434,0.,-0.500000000000007));
#2836=DIRECTION('',(6.32081666887542E-15,0.447213595499956,0.894427190999917));
#2837=DIRECTION('center_axis',(-0.249999999999996,-0.86602540378444,0.433012701892219));
#2838=DIRECTION('ref_axis',(7.449066610202E-18,-0.447213595499957,-0.894427190999916));
#2839=DIRECTION('',(0.866025403784442,0.,0.499999999999995));
#2840=DIRECTION('',(-0.774596669241482,0.447213595499956,0.447213595499962));
#2841=DIRECTION('center_axis',(-0.499999999999998,-0.86602540378444,1.65254605861087E-15));
#2842=DIRECTION('ref_axis',(0.86602540378444,-0.499999999999998,-1.10237170434595E-32));
#2843=DIRECTION('',(3.30509211722174E-15,0.,1.));
#2844=DIRECTION('',(-0.774596669241485,0.447213595499956,-0.447213595499957));
#2845=DIRECTION('center_axis',(-0.249999999999999,-0.86602540378444,-0.433012701892217));
#2846=DIRECTION('ref_axis',(-8.79687280792217E-19,0.447213595499956,-0.894427190999917));
#2847=DIRECTION('',(-0.866025403784438,0.,0.500000000000001));
#2848=DIRECTION('center_axis',(0.,1.,0.));
#2849=DIRECTION('ref_axis',(0.,0.,1.));
#2850=DIRECTION('',(0.,0.,1.));
#2851=DIRECTION('',(1.,0.,0.));
#2852=DIRECTION('',(0.,0.,1.));
#2853=DIRECTION('',(1.,0.,0.));
#2854=DIRECTION('',(1.,0.,0.));
#2855=DIRECTION('',(0.,0.,-1.));
#2856=DIRECTION('',(0.999924833653875,-0.0122607928891601,0.));
#2857=DIRECTION('',(0.,0.,-1.));
#2858=DIRECTION('',(0.,0.,1.));
#2859=DIRECTION('',(1.,0.,0.));
#2860=DIRECTION('',(0.,0.,1.));
#2861=DIRECTION('',(1.,0.,0.));
#2862=DIRECTION('',(-0.525042831656126,-0.851075804453703,0.));
#2863=DIRECTION('',(-0.851075804453703,0.525042831656126,0.));
#2864=DIRECTION('',(1.,0.,0.));
#2865=DIRECTION('',(0.,0.,-1.));
#2866=DIRECTION('',(-7.65359997600967E-15,0.,-1.));
#2867=DIRECTION('',(-1.,0.,7.65359997600967E-15));
#2868=DIRECTION('',(0.,0.,1.));
#2869=DIRECTION('',(1.,0.,0.));
#2870=DIRECTION('',(-1.,0.,0.));
#2871=DIRECTION('',(0.,1.,0.));
#2872=DIRECTION('',(-1.,0.,0.));
#2873=DIRECTION('',(0.,-1.,0.));
#2874=DIRECTION('',(-1.,0.,0.));
#2875=DIRECTION('',(0.,-1.,0.));
#2876=CARTESIAN_POINT('',(0.,0.,0.));
#2877=CARTESIAN_POINT('',(0.,0.,0.));
#2878=CARTESIAN_POINT('Origin',(0.,0.,24.));
#2879=CARTESIAN_POINT('',(7.,-8.57252759403147E-16,24.));
#2880=CARTESIAN_POINT('Origin',(0.,0.,24.));
#2881=CARTESIAN_POINT('',(7.,-8.57252759403147E-16,0.));
#2882=CARTESIAN_POINT('',(7.,-8.57252759403147E-16,24.));
#2883=CARTESIAN_POINT('Origin',(0.,0.,0.));
#2884=CARTESIAN_POINT('Origin',(0.,0.,24.));
#2885=CARTESIAN_POINT('',(9.,-1.10218211923262E-15,0.));
#2886=CARTESIAN_POINT('Origin',(0.,0.,0.));
#2887=CARTESIAN_POINT('',(9.,-1.10218211923262E-15,24.));
#2888=CARTESIAN_POINT('',(9.,-1.10218211923262E-15,24.));
#2889=CARTESIAN_POINT('Origin',(0.,0.,24.));
#2890=CARTESIAN_POINT('Origin',(0.,0.,24.));
#2891=CARTESIAN_POINT('Origin',(0.,0.,0.));
#2892=CARTESIAN_POINT('',(0.,0.,0.));
#2893=CARTESIAN_POINT('Origin',(0.,0.,69.));
#2894=CARTESIAN_POINT('',(-6.,-7.34788079488412E-16,70.));
#2895=CARTESIAN_POINT('Origin',(0.,0.,70.));
#2896=CARTESIAN_POINT('',(-7.,-8.57252759403147E-16,69.));
#2897=CARTESIAN_POINT('Origin',(-6.,-7.34788079488412E-16,69.));
#2898=CARTESIAN_POINT('',(7.,8.57252759403147E-16,69.));
#2899=CARTESIAN_POINT('Origin',(0.,0.,69.));
#2900=CARTESIAN_POINT('Origin',(0.,0.,69.));
#2901=CARTESIAN_POINT('Origin',(0.,0.,1.));
#2902=CARTESIAN_POINT('',(7.,8.57252759403147E-16,1.));
#2903=CARTESIAN_POINT('',(-7.,-8.57252759403147E-16,1.));
#2904=CARTESIAN_POINT('Origin',(0.,0.,1.));
#2905=CARTESIAN_POINT('Origin',(0.,0.,1.));
#2906=CARTESIAN_POINT('',(-6.,-7.34788079488412E-16,0.));
#2907=CARTESIAN_POINT('Origin',(-6.,-7.34788079488412E-16,1.));
#2908=CARTESIAN_POINT('Origin',(0.,0.,0.));
#2909=CARTESIAN_POINT('Origin',(0.,0.,70.));
#2910=CARTESIAN_POINT('',(7.,-8.57252759403147E-16,70.));
#2911=CARTESIAN_POINT('',(-4.89897948556636,5.,4.));
#2912=CARTESIAN_POINT('',(-4.89897948556636,5.,6.00000000000001));
#2913=CARTESIAN_POINT('',(-4.89897948556636,5.,70.));
#2914=CARTESIAN_POINT('',(4.89897948556636,5.,4.));
#2915=CARTESIAN_POINT('Origin',(0.,0.,4.));
#2916=CARTESIAN_POINT('',(4.89897948556636,5.,6.00000000000001));
#2917=CARTESIAN_POINT('',(4.89897948556636,5.,70.));
#2918=CARTESIAN_POINT('Origin',(0.,0.,6.00000000000001));
#2919=CARTESIAN_POINT('',(4.89897948556636,5.,66.));
#2920=CARTESIAN_POINT('',(4.89897948556636,5.,64.));
#2921=CARTESIAN_POINT('',(4.89897948556636,5.,70.));
#2922=CARTESIAN_POINT('',(-4.89897948556636,5.,66.));
#2923=CARTESIAN_POINT('Origin',(0.,0.,66.));
#2924=CARTESIAN_POINT('',(-4.89897948556636,5.,64.));
#2925=CARTESIAN_POINT('',(-4.89897948556636,5.,70.));
#2926=CARTESIAN_POINT('Origin',(0.,0.,64.));
#2927=CARTESIAN_POINT('Origin',(0.,0.,70.));
#2928=CARTESIAN_POINT('Origin',(0.,0.,0.));
#2929=CARTESIAN_POINT('Origin',(2.44929359829471E-16,5.,66.));
#2930=CARTESIAN_POINT('',(2.44929359829471E-16,5.,64.));
#2931=CARTESIAN_POINT('',(-6.13964394045187,5.,66.));
#2932=CARTESIAN_POINT('Origin',(0.,0.,66.));
#2933=CARTESIAN_POINT('Origin',(0.,0.,64.));
#2934=CARTESIAN_POINT('Origin',(-2.44929359829471E-16,5.,4.));
#2935=CARTESIAN_POINT('',(5.87651634300394,5.,4.));
#2936=CARTESIAN_POINT('',(-2.44929359829471E-16,5.,6.));
#2937=CARTESIAN_POINT('Origin',(0.,0.,4.));
#2938=CARTESIAN_POINT('Origin',(0.,0.,6.));
#2939=CARTESIAN_POINT('',(0.,0.,0.));
#2940=CARTESIAN_POINT('Origin',(-2.4980018054066E-13,0.,0.));
#2941=CARTESIAN_POINT('',(-1.86716085299465,4.93327704403918E-15,-40.283264100914));
#2942=CARTESIAN_POINT('Origin',(-1.86716085299465,0.,0.));
#2943=CARTESIAN_POINT('',(1.86716085299415,-4.93327704403918E-15,-40.283264100914));
#2944=CARTESIAN_POINT('Origin',(-2.4980018054066E-13,-5.02105187650471E-15,
-41.0000000000046));
#2945=CARTESIAN_POINT('',(1.86716085299415,5.40579083997353E-15,40.283264100914));
#2946=CARTESIAN_POINT('Origin',(1.86716085299415,0.,0.));
#2947=CARTESIAN_POINT('Origin',(1.86716085299415,0.,0.));
#2948=CARTESIAN_POINT('Origin',(15.,0.,0.));
#2949=CARTESIAN_POINT('',(12.,-1.10218211923262E-15,-9.));
#2950=CARTESIAN_POINT('Origin',(12.,0.,0.));
#2951=CARTESIAN_POINT('',(-11.9999999999937,-1.10218211923262E-15,-9.));
#2952=CARTESIAN_POINT('',(15.,-1.10218211923262E-15,-9.));
#2953=CARTESIAN_POINT('Origin',(-11.9999999999937,0.,0.));
#2954=CARTESIAN_POINT('Origin',(5.0000000000226,0.,0.));
#2955=CARTESIAN_POINT('',(3.0000000000226,-1.95943487863597E-15,-16.0000000000017));
#2956=CARTESIAN_POINT('Origin',(3.0000000000226,0.,0.));
#2957=CARTESIAN_POINT('',(5.0000000000226,-1.71450551880685E-15,-14.0000000000046));
#2958=CARTESIAN_POINT('Origin',(5.0000000000226,-1.95943487863633E-15,-16.0000000000046));
#2959=CARTESIAN_POINT('Origin',(5.0000000000226,0.,0.));
#2960=CARTESIAN_POINT('Origin',(-11.9999999999937,0.,0.));
#2961=CARTESIAN_POINT('',(12.,-1.71450551880685E-15,-14.0000000000046));
#2962=CARTESIAN_POINT('',(-11.9999999999937,-1.71450551880685E-15,-14.0000000000046));
#2963=CARTESIAN_POINT('Origin',(12.,0.,0.));
#2964=CARTESIAN_POINT('Origin',(-11.9999999999937,0.,0.));
#2965=CARTESIAN_POINT('',(-11.9999999999937,-1.71450551880603E-15,-13.9999999999978));
#2966=CARTESIAN_POINT('Origin',(-11.9999999999937,0.,0.));
#2967=CARTESIAN_POINT('',(-4.99999999998797,-1.71450551880603E-15,-13.9999999999978));
#2968=CARTESIAN_POINT('',(-11.9999999999937,-1.71450551880603E-15,-13.9999999999978));
#2969=CARTESIAN_POINT('Origin',(-4.99999999998797,0.,0.));
#2970=CARTESIAN_POINT('Origin',(-4.99999999998797,0.,0.));
#2971=CARTESIAN_POINT('',(-2.99999999998797,-1.9594348786355E-15,-15.9999999999978));
#2972=CARTESIAN_POINT('Origin',(-4.99999999998797,-1.9594348786355E-15,
-15.9999999999978));
#2973=CARTESIAN_POINT('Origin',(-2.99999999998797,0.,0.));
#2974=CARTESIAN_POINT('Origin',(-4.99999999998797,0.,0.));
#2975=CARTESIAN_POINT('',(-2.99999999998797,-4.16379911710073E-15,-33.9999999999978));
#2976=CARTESIAN_POINT('Origin',(-2.99999999998797,0.,0.));
#2977=CARTESIAN_POINT('',(-4.99999999998797,-4.40872847693021E-15,-35.9999999999978));
#2978=CARTESIAN_POINT('Origin',(-4.99999999998797,-4.16379911710073E-15,
-33.9999999999978));
#2979=CARTESIAN_POINT('Origin',(-4.99999999998797,0.,0.));
#2980=CARTESIAN_POINT('Origin',(-11.9999999999937,0.,0.));
#2981=CARTESIAN_POINT('',(-8.99999999999736,-4.40872847693021E-15,-35.9999999999978));
#2982=CARTESIAN_POINT('',(-11.9999999999937,-4.40872847693021E-15,-35.9999999999978));
#2983=CARTESIAN_POINT('Origin',(-8.99999999999736,0.,0.));
#2984=CARTESIAN_POINT('Origin',(-11.9999999999937,0.,0.));
#2985=CARTESIAN_POINT('',(-8.99999999999736,-5.87830463590787E-15,-48.0000000000047));
#2986=CARTESIAN_POINT('Origin',(-8.99999999999736,0.,0.));
#2987=CARTESIAN_POINT('',(-4.82933823252224,-5.87830463590787E-15,-48.0000000000047));
#2988=CARTESIAN_POINT('',(-11.9999999999937,-5.87830463590787E-15,-48.0000000000047));
#2989=CARTESIAN_POINT('Origin',(-4.82933823252224,0.,0.));
#2990=CARTESIAN_POINT('Origin',(-1.86716085299465,0.,0.));
#2991=CARTESIAN_POINT('',(-1.86716085299465,-4.93327704403918E-15,-40.283264100914));
#2992=CARTESIAN_POINT('Origin',(1.86716085299415,0.,0.));
#2993=CARTESIAN_POINT('',(4.82933823252174,5.87830463590787E-15,-48.0000000000047));
#2994=CARTESIAN_POINT('',(4.82933823252174,-5.87830463590787E-15,48.0000000000047));
#2995=CARTESIAN_POINT('Origin',(4.82933823252174,0.,0.));
#2996=CARTESIAN_POINT('',(1.86716085299415,-4.93327704403918E-15,40.283264100914));
#2997=CARTESIAN_POINT('Origin',(4.82933823252174,0.,0.));
#2998=CARTESIAN_POINT('Origin',(-11.9999999999937,0.,0.));
#2999=CARTESIAN_POINT('',(9.00000000000556,-5.87830463590787E-15,-48.0000000000047));
#3000=CARTESIAN_POINT('',(-11.9999999999937,-5.87830463590787E-15,-48.0000000000047));
#3001=CARTESIAN_POINT('Origin',(9.00000000000556,0.,0.));
#3002=CARTESIAN_POINT('Origin',(-11.9999999999937,0.,0.));
#3003=CARTESIAN_POINT('',(9.00000000000556,-4.40872847693068E-15,-36.0000000000017));
#3004=CARTESIAN_POINT('Origin',(9.00000000000556,0.,0.));
#3005=CARTESIAN_POINT('',(5.0000000000226,-4.40872847693068E-15,-36.0000000000017));
#3006=CARTESIAN_POINT('',(-11.9999999999937,-4.40872847693068E-15,-36.0000000000017));
#3007=CARTESIAN_POINT('Origin',(5.0000000000226,0.,0.));
#3008=CARTESIAN_POINT('Origin',(5.0000000000226,0.,0.));
#3009=CARTESIAN_POINT('',(3.0000000000226,-4.16379911710121E-15,-34.0000000000017));
#3010=CARTESIAN_POINT('Origin',(5.0000000000226,-4.16379911710121E-15,-34.0000000000017));
#3011=CARTESIAN_POINT('Origin',(3.0000000000226,0.,0.));
#3012=CARTESIAN_POINT('Origin',(-11.9999999999937,0.,0.));
#3013=CARTESIAN_POINT('Origin',(12.,0.,0.));
#3014=CARTESIAN_POINT('Origin',(3.0000000000226,0.,0.));
#3015=CARTESIAN_POINT('Origin',(9.00000000000556,0.,0.));
#3016=CARTESIAN_POINT('Origin',(-8.99999999999736,0.,0.));
#3017=CARTESIAN_POINT('Origin',(-2.99999999998797,0.,0.));
#3018=CARTESIAN_POINT('',(0.,0.,0.));
#3019=CARTESIAN_POINT('Origin',(-5.,0.,0.));
#3020=CARTESIAN_POINT('',(5.,-8.57252759403147E-16,-7.));
#3021=CARTESIAN_POINT('Origin',(5.,0.,0.));
#3022=CARTESIAN_POINT('',(-5.,-8.57252759403147E-16,-7.));
#3023=CARTESIAN_POINT('',(-5.,-8.57252759403147E-16,-7.));
#3024=CARTESIAN_POINT('Origin',(-5.,0.,0.));
#3025=CARTESIAN_POINT('Origin',(-5.,0.,0.));
#3026=CARTESIAN_POINT('',(-5.,-1.46957615897682E-15,-12.));
#3027=CARTESIAN_POINT('Origin',(-5.,0.,0.));
#3028=CARTESIAN_POINT('',(5.,-1.46957615897682E-15,-12.));
#3029=CARTESIAN_POINT('',(-5.,-1.46957615897682E-15,-12.));
#3030=CARTESIAN_POINT('Origin',(5.,0.,0.));
#3031=CARTESIAN_POINT('Origin',(-5.,0.,0.));
#3032=CARTESIAN_POINT('Origin',(5.,0.,0.));
#3033=CARTESIAN_POINT('',(0.,0.,0.));
#3034=CARTESIAN_POINT('Origin',(-0.506247771123191,-14.,18.0160339934195));
#3035=CARTESIAN_POINT('',(-0.506247771123192,-18.,22.0160339934195));
#3036=CARTESIAN_POINT('Origin',(-0.506247771123191,-18.,18.0160339934195));
#3037=CARTESIAN_POINT('',(-0.506247771123192,-24.,22.0160339934195));
#3038=CARTESIAN_POINT('',(-0.506247771123192,-14.,22.0160339934195));
#3039=CARTESIAN_POINT('Origin',(-0.506247771123191,-24.,18.0160339934195));
#3040=CARTESIAN_POINT('Origin',(-11.,9.00000000000001,0.));
#3041=CARTESIAN_POINT('',(-9.35000000000001,9.00000000000001,7.));
#3042=CARTESIAN_POINT('Origin',(-11.,9.00000000000001,7.));
#3043=CARTESIAN_POINT('',(-9.35000000000001,9.00000000000001,-1.35323471305782E-15));
#3044=CARTESIAN_POINT('',(-9.35000000000001,9.00000000000001,0.));
#3045=CARTESIAN_POINT('Origin',(-11.,9.00000000000001,-1.35323471305782E-15));
#3046=CARTESIAN_POINT('Origin',(11.,9.,0.));
#3047=CARTESIAN_POINT('',(12.65,9.,7.));
#3048=CARTESIAN_POINT('Origin',(11.,9.,7.));
#3049=CARTESIAN_POINT('',(12.65,9.,-1.35323471305782E-15));
#3050=CARTESIAN_POINT('',(12.65,9.,0.));
#3051=CARTESIAN_POINT('Origin',(11.,9.,-1.35323471305782E-15));
#3052=CARTESIAN_POINT('Origin',(0.,-2.5,9.99999999999999));
#3053=CARTESIAN_POINT('',(7.,-2.5,7.));
#3054=CARTESIAN_POINT('Origin',(0.,-2.5,7.));
#3055=CARTESIAN_POINT('',(7.,-2.5,-1.11022302462516E-15));
#3056=CARTESIAN_POINT('',(7.,-2.5,9.99999999999999));
#3057=CARTESIAN_POINT('Origin',(0.,-2.5,0.));
#3058=CARTESIAN_POINT('Origin',(0.,0.,7.));
#3059=CARTESIAN_POINT('',(-20.,18.,7.));
#3060=CARTESIAN_POINT('',(-20.,-18.,7.));
#3061=CARTESIAN_POINT('',(-20.,24.,7.));
#3062=CARTESIAN_POINT('',(20.,-18.,7.));
#3063=CARTESIAN_POINT('',(-20.,-18.,7.));
#3064=CARTESIAN_POINT('',(20.,18.,7.));
#3065=CARTESIAN_POINT('',(20.,-24.,7.));
#3066=CARTESIAN_POINT('',(-20.,18.,7.));
#3067=CARTESIAN_POINT('Origin',(2.93915231795365E-15,-24.,7.));
#3068=CARTESIAN_POINT('',(-20.,-24.,0.));
#3069=CARTESIAN_POINT('',(20.,-24.,0.));
#3070=CARTESIAN_POINT('',(2.93915231795365E-15,-24.,0.));
#3071=CARTESIAN_POINT('',(20.,-24.,26.));
#3072=CARTESIAN_POINT('',(20.,-24.,7.));
#3073=CARTESIAN_POINT('',(-20.,-24.,26.));
#3074=CARTESIAN_POINT('',(20.,-24.,26.));
#3075=CARTESIAN_POINT('',(-20.,-24.,7.));
#3076=CARTESIAN_POINT('Origin',(20.,-24.,7.));
#3077=CARTESIAN_POINT('',(20.,24.,0.));
#3078=CARTESIAN_POINT('',(20.,-24.,0.));
#3079=CARTESIAN_POINT('',(20.,24.,26.));
#3080=CARTESIAN_POINT('',(20.,24.,7.));
#3081=CARTESIAN_POINT('',(20.,18.,26.));
#3082=CARTESIAN_POINT('',(20.,18.,26.));
#3083=CARTESIAN_POINT('',(20.,18.,26.));
#3084=CARTESIAN_POINT('',(20.,-18.,26.));
#3085=CARTESIAN_POINT('',(20.,-18.,26.));
#3086=CARTESIAN_POINT('',(20.,-18.,26.));
#3087=CARTESIAN_POINT('Origin',(20.,24.,7.));
#3088=CARTESIAN_POINT('',(-20.,24.,0.));
#3089=CARTESIAN_POINT('',(20.,24.,0.));
#3090=CARTESIAN_POINT('',(-20.,24.,26.));
#3091=CARTESIAN_POINT('',(-20.,24.,7.));
#3092=CARTESIAN_POINT('',(20.,24.,26.));
#3093=CARTESIAN_POINT('Origin',(-20.,24.,7.));
#3094=CARTESIAN_POINT('',(-20.,24.,0.));
#3095=CARTESIAN_POINT('',(-20.,-18.,26.));
#3096=CARTESIAN_POINT('',(-20.,-24.,26.));
#3097=CARTESIAN_POINT('',(-20.,-18.,26.));
#3098=CARTESIAN_POINT('',(-20.,18.,26.));
#3099=CARTESIAN_POINT('',(-20.,18.,26.));
#3100=CARTESIAN_POINT('',(-20.,24.,26.));
#3101=CARTESIAN_POINT('Origin',(0.,0.,0.));
#3102=CARTESIAN_POINT('Origin',(-20.,18.,26.));
#3103=CARTESIAN_POINT('',(-20.,18.,26.));
#3104=CARTESIAN_POINT('Origin',(0.,0.,26.));
#3105=CARTESIAN_POINT('Origin',(-20.,-18.,26.));
#3106=CARTESIAN_POINT('',(-20.,-18.,26.));
#3107=CARTESIAN_POINT('Origin',(0.,0.,26.));
#3108=CARTESIAN_POINT('',(0.,0.,0.));
#3109=CARTESIAN_POINT('Origin',(28.,6.5,2.));
#3110=CARTESIAN_POINT('',(30.125,6.5,2.));
#3111=CARTESIAN_POINT('Origin',(28.,6.5,2.));
#3112=CARTESIAN_POINT('',(30.125,6.5,0.));
#3113=CARTESIAN_POINT('',(30.125,6.5,2.));
#3114=CARTESIAN_POINT('Origin',(28.,6.5,0.));
#3115=CARTESIAN_POINT('Origin',(6.,6.5,2.));
#3116=CARTESIAN_POINT('',(8.25,6.5,2.));
#3117=CARTESIAN_POINT('Origin',(6.,6.5,2.));
#3118=CARTESIAN_POINT('',(8.25,6.5,0.));
#3119=CARTESIAN_POINT('',(8.25,6.5,2.));
#3120=CARTESIAN_POINT('Origin',(6.,6.5,0.));
#3121=CARTESIAN_POINT('Origin',(0.,0.,2.));
#3122=CARTESIAN_POINT('',(0.,11.,2.));
#3123=CARTESIAN_POINT('',(0.,0.,2.));
#3124=CARTESIAN_POINT('',(0.,11.,2.));
#3125=CARTESIAN_POINT('',(34.,0.,2.));
#3126=CARTESIAN_POINT('',(0.,0.,2.));
#3127=CARTESIAN_POINT('',(34.,11.,2.));
#3128=CARTESIAN_POINT('',(34.,0.,2.));
#3129=CARTESIAN_POINT('',(34.,11.,2.));
#3130=CARTESIAN_POINT('Origin',(0.,0.,0.));
#3131=CARTESIAN_POINT('',(0.,11.,0.));
#3132=CARTESIAN_POINT('',(0.,0.,0.));
#3133=CARTESIAN_POINT('',(0.,11.,0.));
#3134=CARTESIAN_POINT('',(34.,11.,0.));
#3135=CARTESIAN_POINT('',(34.,11.,0.));
#3136=CARTESIAN_POINT('',(34.,0.,0.));
#3137=CARTESIAN_POINT('',(34.,0.,0.));
#3138=CARTESIAN_POINT('',(0.,0.,0.));
#3139=CARTESIAN_POINT('Origin',(0.,11.,2.));
#3140=CARTESIAN_POINT('',(0.,0.,2.));
#3141=CARTESIAN_POINT('',(0.,11.,2.));
#3142=CARTESIAN_POINT('Origin',(0.,0.,2.));
#3143=CARTESIAN_POINT('',(34.,0.,2.));
#3144=CARTESIAN_POINT('Origin',(34.,0.,2.));
#3145=CARTESIAN_POINT('',(34.,11.,2.));
#3146=CARTESIAN_POINT('Origin',(34.,11.,2.));
#3147=CARTESIAN_POINT('',(0.,0.,0.));
#3148=CARTESIAN_POINT('Origin',(-2.77555756156289E-16,71.6937500009559,
-2.08166817117217E-16));
#3149=CARTESIAN_POINT('',(1.6211138875,8.95625000095593,-2.08166817117217E-16));
#3150=CARTESIAN_POINT('',(1.6211138875,9.13125000095592,-2.08166817117217E-16));
#3151=CARTESIAN_POINT('',(1.6211138875,71.6937500009559,-2.17804440896414E-16));
#3152=CARTESIAN_POINT('',(0.538440894222362,9.51999998211971,1.52908195976357));
#3153=CARTESIAN_POINT('Ctrl Pts',(0.538440894222362,9.51999996467551,1.52908195976357));
#3154=CARTESIAN_POINT('Ctrl Pts',(-0.164839976619388,9.46938696606746,1.77673067379592));
#3155=CARTESIAN_POINT('Ctrl Pts',(-0.810556943749999,9.42291666762259,1.40392580900275));
#3156=CARTESIAN_POINT('Ctrl Pts',(-1.6211138875,9.36458333428926,0.935950539335167));
#3157=CARTESIAN_POINT('Ctrl Pts',(-1.6211138875,9.30625000095593,0.));
#3158=CARTESIAN_POINT('Ctrl Pts',(-1.6211138875,9.24791666762259,-0.935950539335166));
#3159=CARTESIAN_POINT('Ctrl Pts',(-0.81055694375,9.18958333428926,-1.40392580900275));
#3160=CARTESIAN_POINT('Ctrl Pts',(-1.14620883215705E-16,9.13125000095592,
-1.87190107867033));
#3161=CARTESIAN_POINT('Ctrl Pts',(0.81055694375,9.0729166676226,-1.40392580900275));
#3162=CARTESIAN_POINT('Ctrl Pts',(1.6211138875,9.01458333428926,-0.935950539335166));
#3163=CARTESIAN_POINT('Ctrl Pts',(1.6211138875,8.95625000095593,-1.9852919333802E-16));
#3164=CARTESIAN_POINT('',(-1.52006374725761,9.52000000000001,0.563397231550268));
#3165=CARTESIAN_POINT('Origin',(-2.77555756156289E-16,9.52000000000001,
-2.08166817117217E-16));
#3166=CARTESIAN_POINT('Ctrl Pts',(-1.52006374725761,9.52000000000001,0.563397231550268));
#3167=CARTESIAN_POINT('Ctrl Pts',(-1.6211138875,9.49937173003197,0.290760721755766));
#3168=CARTESIAN_POINT('Ctrl Pts',(-1.6211138875,9.48125000095592,0.));
#3169=CARTESIAN_POINT('Ctrl Pts',(-1.6211138875,9.42291666762259,-0.935950539335166));
#3170=CARTESIAN_POINT('Ctrl Pts',(-0.81055694375,9.36458333428925,-1.40392580900275));
#3171=CARTESIAN_POINT('Ctrl Pts',(-1.14620883215705E-16,9.30625000095592,
-1.87190107867033));
#3172=CARTESIAN_POINT('Ctrl Pts',(0.81055694375,9.24791666762259,-1.40392580900275));
#3173=CARTESIAN_POINT('Ctrl Pts',(1.6211138875,9.18958333428925,-0.935950539335166));
#3174=CARTESIAN_POINT('Ctrl Pts',(1.6211138875,9.13125000095592,-1.9852919333802E-16));
#3175=CARTESIAN_POINT('Origin',(-2.77555756156289E-16,71.6937500009559,
-2.08166817117217E-16));
#3176=CARTESIAN_POINT('',(1.6211138875,8.25625000095592,-2.08166817117217E-16));
#3177=CARTESIAN_POINT('',(1.6211138875,8.43125000095592,-2.08166817117217E-16));
#3178=CARTESIAN_POINT('',(1.6211138875,71.6937500009559,-2.17804440896414E-16));
#3179=CARTESIAN_POINT('Ctrl Pts',(1.6211138875,8.95625000095593,-1.9852919333802E-16));
#3180=CARTESIAN_POINT('Ctrl Pts',(1.6211138875,8.89791666762259,0.935950539335165));
#3181=CARTESIAN_POINT('Ctrl Pts',(0.810556943750001,8.83958333428926,1.40392580900275));
#3182=CARTESIAN_POINT('Ctrl Pts',(3.43862649647115E-16,8.78125000095592,
1.87190107867033));
#3183=CARTESIAN_POINT('Ctrl Pts',(-0.810556943749999,8.72291666762259,1.40392580900275));
#3184=CARTESIAN_POINT('Ctrl Pts',(-1.6211138875,8.66458333428927,0.935950539335167));
#3185=CARTESIAN_POINT('Ctrl Pts',(-1.6211138875,8.60625000095593,0.));
#3186=CARTESIAN_POINT('Ctrl Pts',(-1.6211138875,8.5479166676226,-0.935950539335166));
#3187=CARTESIAN_POINT('Ctrl Pts',(-0.81055694375,8.48958333428926,-1.40392580900275));
#3188=CARTESIAN_POINT('Ctrl Pts',(-1.14620883215705E-16,8.43125000095593,
-1.87190107867033));
#3189=CARTESIAN_POINT('Ctrl Pts',(0.81055694375,8.37291666762259,-1.40392580900275));
#3190=CARTESIAN_POINT('Ctrl Pts',(1.6211138875,8.31458333428926,-0.935950539335166));
#3191=CARTESIAN_POINT('Ctrl Pts',(1.6211138875,8.25625000095592,-1.9852919333802E-16));
#3192=CARTESIAN_POINT('Ctrl Pts',(1.6211138875,9.13125000095592,-1.9852919333802E-16));
#3193=CARTESIAN_POINT('Ctrl Pts',(1.6211138875,9.07291666762258,0.935950539335165));
#3194=CARTESIAN_POINT('Ctrl Pts',(0.810556943750001,9.01458333428926,1.40392580900275));
#3195=CARTESIAN_POINT('Ctrl Pts',(3.43862649647115E-16,8.95625000095592,
1.87190107867033));
#3196=CARTESIAN_POINT('Ctrl Pts',(-0.810556943749999,8.89791666762259,1.40392580900275));
#3197=CARTESIAN_POINT('Ctrl Pts',(-1.6211138875,8.83958333428926,0.935950539335167));
#3198=CARTESIAN_POINT('Ctrl Pts',(-1.6211138875,8.78125000095592,0.));
#3199=CARTESIAN_POINT('Ctrl Pts',(-1.6211138875,8.72291666762259,-0.935950539335166));
#3200=CARTESIAN_POINT('Ctrl Pts',(-0.81055694375,8.66458333428925,-1.40392580900275));
#3201=CARTESIAN_POINT('Ctrl Pts',(-1.14620883215705E-16,8.60625000095593,
-1.87190107867033));
#3202=CARTESIAN_POINT('Ctrl Pts',(0.81055694375,8.54791666762259,-1.40392580900275));
#3203=CARTESIAN_POINT('Ctrl Pts',(1.6211138875,8.48958333428926,-0.935950539335166));
#3204=CARTESIAN_POINT('Ctrl Pts',(1.6211138875,8.43125000095592,-1.9852919333802E-16));
#3205=CARTESIAN_POINT('Origin',(-2.77555756156289E-16,71.6937500009559,
-2.08166817117217E-16));
#3206=CARTESIAN_POINT('',(1.6211138875,7.55625000095593,-2.08166817117217E-16));
#3207=CARTESIAN_POINT('',(1.6211138875,7.73125000095592,-2.08166817117217E-16));
#3208=CARTESIAN_POINT('',(1.6211138875,71.6937500009559,-2.17804440896414E-16));
#3209=CARTESIAN_POINT('Ctrl Pts',(1.6211138875,8.25625000095592,-1.9852919333802E-16));
#3210=CARTESIAN_POINT('Ctrl Pts',(1.6211138875,8.1979166676226,0.935950539335165));
#3211=CARTESIAN_POINT('Ctrl Pts',(0.810556943750001,8.13958333428925,1.40392580900275));
#3212=CARTESIAN_POINT('Ctrl Pts',(3.43862649647115E-16,8.08125000095593,
1.87190107867033));
#3213=CARTESIAN_POINT('Ctrl Pts',(-0.810556943749999,8.02291666762259,1.40392580900275));
#3214=CARTESIAN_POINT('Ctrl Pts',(-1.6211138875,7.96458333428926,0.935950539335167));
#3215=CARTESIAN_POINT('Ctrl Pts',(-1.6211138875,7.90625000095593,0.));
#3216=CARTESIAN_POINT('Ctrl Pts',(-1.6211138875,7.84791666762259,-0.935950539335166));
#3217=CARTESIAN_POINT('Ctrl Pts',(-0.81055694375,7.78958333428927,-1.40392580900275));
#3218=CARTESIAN_POINT('Ctrl Pts',(-1.14620883215705E-16,7.73125000095592,
-1.87190107867033));
#3219=CARTESIAN_POINT('Ctrl Pts',(0.81055694375,7.6729166676226,-1.40392580900275));
#3220=CARTESIAN_POINT('Ctrl Pts',(1.6211138875,7.61458333428926,-0.935950539335166));
#3221=CARTESIAN_POINT('Ctrl Pts',(1.6211138875,7.55625000095593,-1.9852919333802E-16));
#3222=CARTESIAN_POINT('Ctrl Pts',(1.6211138875,8.43125000095592,-1.9852919333802E-16));
#3223=CARTESIAN_POINT('Ctrl Pts',(1.6211138875,8.37291666762259,0.935950539335165));
#3224=CARTESIAN_POINT('Ctrl Pts',(0.810556943750001,8.31458333428925,1.40392580900275));
#3225=CARTESIAN_POINT('Ctrl Pts',(3.43862649647115E-16,8.25625000095592,
1.87190107867033));
#3226=CARTESIAN_POINT('Ctrl Pts',(-0.810556943749999,8.19791666762258,1.40392580900275));
#3227=CARTESIAN_POINT('Ctrl Pts',(-1.6211138875,8.13958333428925,0.935950539335167));
#3228=CARTESIAN_POINT('Ctrl Pts',(-1.6211138875,8.08125000095593,0.));
#3229=CARTESIAN_POINT('Ctrl Pts',(-1.6211138875,8.02291666762259,-0.935950539335166));
#3230=CARTESIAN_POINT('Ctrl Pts',(-0.81055694375,7.96458333428926,-1.40392580900275));
#3231=CARTESIAN_POINT('Ctrl Pts',(-1.14620883215705E-16,7.90625000095592,
-1.87190107867033));
#3232=CARTESIAN_POINT('Ctrl Pts',(0.81055694375,7.84791666762259,-1.40392580900275));
#3233=CARTESIAN_POINT('Ctrl Pts',(1.6211138875,7.78958333428925,-0.935950539335166));
#3234=CARTESIAN_POINT('Ctrl Pts',(1.6211138875,7.73125000095592,-1.9852919333802E-16));
#3235=CARTESIAN_POINT('Origin',(-2.77555756156289E-16,71.6937500009559,
-2.08166817117217E-16));
#3236=CARTESIAN_POINT('',(1.6211138875,6.85625000095592,-2.08166817117217E-16));
#3237=CARTESIAN_POINT('',(1.6211138875,7.03125000095592,-2.08166817117217E-16));
#3238=CARTESIAN_POINT('',(1.6211138875,71.6937500009559,-2.17804440896414E-16));
#3239=CARTESIAN_POINT('Ctrl Pts',(1.6211138875,7.55625000095593,-1.9852919333802E-16));
#3240=CARTESIAN_POINT('Ctrl Pts',(1.6211138875,7.49791666762259,0.935950539335165));
#3241=CARTESIAN_POINT('Ctrl Pts',(0.810556943750001,7.43958333428926,1.40392580900275));
#3242=CARTESIAN_POINT('Ctrl Pts',(3.43862649647115E-16,7.38125000095592,
1.87190107867033));
#3243=CARTESIAN_POINT('Ctrl Pts',(-0.810556943749999,7.3229166676226,1.40392580900275));
#3244=CARTESIAN_POINT('Ctrl Pts',(-1.6211138875,7.26458333428925,0.935950539335167));
#3245=CARTESIAN_POINT('Ctrl Pts',(-1.6211138875,7.20625000095593,0.));
#3246=CARTESIAN_POINT('Ctrl Pts',(-1.6211138875,7.1479166676226,-0.935950539335166));
#3247=CARTESIAN_POINT('Ctrl Pts',(-0.81055694375,7.08958333428926,-1.40392580900275));
#3248=CARTESIAN_POINT('Ctrl Pts',(-1.14620883215705E-16,7.03125000095593,
-1.87190107867033));
#3249=CARTESIAN_POINT('Ctrl Pts',(0.81055694375,6.97291666762259,-1.40392580900275));
#3250=CARTESIAN_POINT('Ctrl Pts',(1.6211138875,6.91458333428927,-0.935950539335166));
#3251=CARTESIAN_POINT('Ctrl Pts',(1.6211138875,6.85625000095592,-1.9852919333802E-16));
#3252=CARTESIAN_POINT('Ctrl Pts',(1.6211138875,7.73125000095592,-1.9852919333802E-16));
#3253=CARTESIAN_POINT('Ctrl Pts',(1.6211138875,7.67291666762258,0.935950539335165));
#3254=CARTESIAN_POINT('Ctrl Pts',(0.810556943750001,7.61458333428926,1.40392580900275));
#3255=CARTESIAN_POINT('Ctrl Pts',(3.43862649647115E-16,7.55625000095592,
1.87190107867033));
#3256=CARTESIAN_POINT('Ctrl Pts',(-0.810556943749999,7.49791666762259,1.40392580900275));
#3257=CARTESIAN_POINT('Ctrl Pts',(-1.6211138875,7.43958333428925,0.935950539335167));
#3258=CARTESIAN_POINT('Ctrl Pts',(-1.6211138875,7.38125000095592,0.));
#3259=CARTESIAN_POINT('Ctrl Pts',(-1.6211138875,7.3229166676226,-0.935950539335166));
#3260=CARTESIAN_POINT('Ctrl Pts',(-0.81055694375,7.26458333428925,-1.40392580900275));
#3261=CARTESIAN_POINT('Ctrl Pts',(-1.14620883215705E-16,7.20625000095593,
-1.87190107867033));
#3262=CARTESIAN_POINT('Ctrl Pts',(0.81055694375,7.14791666762259,-1.40392580900275));
#3263=CARTESIAN_POINT('Ctrl Pts',(1.6211138875,7.08958333428926,-0.935950539335166));
#3264=CARTESIAN_POINT('Ctrl Pts',(1.6211138875,7.03125000095592,-1.9852919333802E-16));
#3265=CARTESIAN_POINT('Origin',(-2.77555756156289E-16,71.6937500009559,
-2.08166817117217E-16));
#3266=CARTESIAN_POINT('',(1.6211138875,6.15625000095593,-2.08166817117217E-16));
#3267=CARTESIAN_POINT('',(1.6211138875,6.33125000095593,-2.08166817117217E-16));
#3268=CARTESIAN_POINT('',(1.6211138875,71.6937500009559,-2.17804440896414E-16));
#3269=CARTESIAN_POINT('Ctrl Pts',(1.6211138875,6.85625000095592,-1.9852919333802E-16));
#3270=CARTESIAN_POINT('Ctrl Pts',(1.6211138875,6.7979166676226,0.935950539335165));
#3271=CARTESIAN_POINT('Ctrl Pts',(0.810556943750001,6.73958333428926,1.40392580900275));
#3272=CARTESIAN_POINT('Ctrl Pts',(3.43862649647115E-16,6.68125000095593,
1.87190107867033));
#3273=CARTESIAN_POINT('Ctrl Pts',(-0.810556943749999,6.62291666762259,1.40392580900275));
#3274=CARTESIAN_POINT('Ctrl Pts',(-1.6211138875,6.56458333428926,0.935950539335167));
#3275=CARTESIAN_POINT('Ctrl Pts',(-1.6211138875,6.50625000095592,0.));
#3276=CARTESIAN_POINT('Ctrl Pts',(-1.6211138875,6.44791666762259,-0.935950539335166));
#3277=CARTESIAN_POINT('Ctrl Pts',(-0.81055694375,6.38958333428925,-1.40392580900275));
#3278=CARTESIAN_POINT('Ctrl Pts',(-1.14620883215705E-16,6.33125000095593,
-1.87190107867033));
#3279=CARTESIAN_POINT('Ctrl Pts',(0.81055694375,6.2729166676226,-1.40392580900275));
#3280=CARTESIAN_POINT('Ctrl Pts',(1.6211138875,6.21458333428926,-0.935950539335166));
#3281=CARTESIAN_POINT('Ctrl Pts',(1.6211138875,6.15625000095593,-1.9852919333802E-16));
#3282=CARTESIAN_POINT('Ctrl Pts',(1.6211138875,7.03125000095592,-1.9852919333802E-16));
#3283=CARTESIAN_POINT('Ctrl Pts',(1.6211138875,6.97291666762259,0.935950539335165));
#3284=CARTESIAN_POINT('Ctrl Pts',(0.810556943750001,6.91458333428925,1.40392580900275));
#3285=CARTESIAN_POINT('Ctrl Pts',(3.43862649647115E-16,6.85625000095592,
1.87190107867033));
#3286=CARTESIAN_POINT('Ctrl Pts',(-0.810556943749999,6.79791666762258,1.40392580900275));
#3287=CARTESIAN_POINT('Ctrl Pts',(-1.6211138875,6.73958333428926,0.935950539335167));
#3288=CARTESIAN_POINT('Ctrl Pts',(-1.6211138875,6.68125000095592,0.));
#3289=CARTESIAN_POINT('Ctrl Pts',(-1.6211138875,6.62291666762259,-0.935950539335166));
#3290=CARTESIAN_POINT('Ctrl Pts',(-0.81055694375,6.56458333428925,-1.40392580900275));
#3291=CARTESIAN_POINT('Ctrl Pts',(-1.14620883215705E-16,6.50625000095592,
-1.87190107867033));
#3292=CARTESIAN_POINT('Ctrl Pts',(0.81055694375,6.44791666762259,-1.40392580900275));
#3293=CARTESIAN_POINT('Ctrl Pts',(1.6211138875,6.38958333428925,-0.935950539335166));
#3294=CARTESIAN_POINT('Ctrl Pts',(1.6211138875,6.33125000095593,-1.9852919333802E-16));
#3295=CARTESIAN_POINT('Origin',(-2.77555756156289E-16,71.6937500009559,
-2.08166817117217E-16));
#3296=CARTESIAN_POINT('',(1.6211138875,5.45625000095593,-2.08166817117217E-16));
#3297=CARTESIAN_POINT('',(1.6211138875,5.63125000095592,-2.08166817117217E-16));
#3298=CARTESIAN_POINT('',(1.6211138875,71.6937500009559,-2.17804440896414E-16));
#3299=CARTESIAN_POINT('Ctrl Pts',(1.6211138875,6.15625000095593,-1.9852919333802E-16));
#3300=CARTESIAN_POINT('Ctrl Pts',(1.6211138875,6.09791666762259,0.935950539335165));
#3301=CARTESIAN_POINT('Ctrl Pts',(0.810556943750001,6.03958333428927,1.40392580900275));
#3302=CARTESIAN_POINT('Ctrl Pts',(3.43862649647115E-16,5.98125000095592,
1.87190107867033));
#3303=CARTESIAN_POINT('Ctrl Pts',(-0.810556943749999,5.9229166676226,1.40392580900275));
#3304=CARTESIAN_POINT('Ctrl Pts',(-1.6211138875,5.86458333428926,0.935950539335167));
#3305=CARTESIAN_POINT('Ctrl Pts',(-1.6211138875,5.80625000095593,0.));
#3306=CARTESIAN_POINT('Ctrl Pts',(-1.6211138875,5.74791666762259,-0.935950539335166));
#3307=CARTESIAN_POINT('Ctrl Pts',(-0.81055694375,5.68958333428926,-1.40392580900275));
#3308=CARTESIAN_POINT('Ctrl Pts',(-1.14620883215705E-16,5.63125000095592,
-1.87190107867033));
#3309=CARTESIAN_POINT('Ctrl Pts',(0.81055694375,5.57291666762259,-1.40392580900275));
#3310=CARTESIAN_POINT('Ctrl Pts',(1.6211138875,5.51458333428927,-0.935950539335166));
#3311=CARTESIAN_POINT('Ctrl Pts',(1.6211138875,5.45625000095593,-1.9852919333802E-16));
#3312=CARTESIAN_POINT('Ctrl Pts',(1.6211138875,6.33125000095593,-1.9852919333802E-16));
#3313=CARTESIAN_POINT('Ctrl Pts',(1.6211138875,6.27291666762259,0.935950539335165));
#3314=CARTESIAN_POINT('Ctrl Pts',(0.810556943750001,6.21458333428926,1.40392580900275));
#3315=CARTESIAN_POINT('Ctrl Pts',(3.43862649647115E-16,6.15625000095592,
1.87190107867033));
#3316=CARTESIAN_POINT('Ctrl Pts',(-0.810556943749999,6.09791666762259,1.40392580900275));
#3317=CARTESIAN_POINT('Ctrl Pts',(-1.6211138875,6.03958333428925,0.935950539335167));
#3318=CARTESIAN_POINT('Ctrl Pts',(-1.6211138875,5.98125000095592,0.));
#3319=CARTESIAN_POINT('Ctrl Pts',(-1.6211138875,5.92291666762258,-0.935950539335166));
#3320=CARTESIAN_POINT('Ctrl Pts',(-0.81055694375,5.86458333428926,-1.40392580900275));
#3321=CARTESIAN_POINT('Ctrl Pts',(-1.14620883215705E-16,5.80625000095591,
-1.87190107867033));
#3322=CARTESIAN_POINT('Ctrl Pts',(0.81055694375,5.74791666762259,-1.40392580900275));
#3323=CARTESIAN_POINT('Ctrl Pts',(1.6211138875,5.68958333428926,-0.935950539335166));
#3324=CARTESIAN_POINT('Ctrl Pts',(1.6211138875,5.63125000095592,-1.9852919333802E-16));
#3325=CARTESIAN_POINT('Origin',(-2.77555756156289E-16,71.6937500009559,
-2.08166817117217E-16));
#3326=CARTESIAN_POINT('',(1.6211138875,4.75625000095593,-2.08166817117217E-16));
#3327=CARTESIAN_POINT('',(1.6211138875,4.93125000095593,-2.08166817117217E-16));
#3328=CARTESIAN_POINT('',(1.6211138875,71.6937500009559,-2.17804440896414E-16));
#3329=CARTESIAN_POINT('Ctrl Pts',(1.6211138875,5.45625000095593,-1.9852919333802E-16));
#3330=CARTESIAN_POINT('Ctrl Pts',(1.6211138875,5.3979166676226,0.935950539335165));
#3331=CARTESIAN_POINT('Ctrl Pts',(0.810556943750001,5.33958333428926,1.40392580900275));
#3332=CARTESIAN_POINT('Ctrl Pts',(3.43862649647115E-16,5.28125000095593,
1.87190107867033));
#3333=CARTESIAN_POINT('Ctrl Pts',(-0.810556943749999,5.22291666762259,1.40392580900275));
#3334=CARTESIAN_POINT('Ctrl Pts',(-1.6211138875,5.16458333428926,0.935950539335167));
#3335=CARTESIAN_POINT('Ctrl Pts',(-1.6211138875,5.10625000095592,0.));
#3336=CARTESIAN_POINT('Ctrl Pts',(-1.6211138875,5.0479166676226,-0.935950539335166));
#3337=CARTESIAN_POINT('Ctrl Pts',(-0.81055694375,4.98958333428925,-1.40392580900275));
#3338=CARTESIAN_POINT('Ctrl Pts',(-1.14620883215705E-16,4.93125000095593,
-1.87190107867033));
#3339=CARTESIAN_POINT('Ctrl Pts',(0.81055694375,4.87291666762259,-1.40392580900275));
#3340=CARTESIAN_POINT('Ctrl Pts',(1.6211138875,4.81458333428926,-0.935950539335166));
#3341=CARTESIAN_POINT('Ctrl Pts',(1.6211138875,4.75625000095593,-1.9852919333802E-16));
#3342=CARTESIAN_POINT('Ctrl Pts',(1.6211138875,5.63125000095592,-1.9852919333802E-16));
#3343=CARTESIAN_POINT('Ctrl Pts',(1.6211138875,5.57291666762259,0.935950539335165));
#3344=CARTESIAN_POINT('Ctrl Pts',(0.810556943750001,5.51458333428925,1.40392580900275));
#3345=CARTESIAN_POINT('Ctrl Pts',(3.43862649647115E-16,5.45625000095593,
1.87190107867033));
#3346=CARTESIAN_POINT('Ctrl Pts',(-0.810556943749999,5.39791666762259,1.40392580900275));
#3347=CARTESIAN_POINT('Ctrl Pts',(-1.6211138875,5.33958333428926,0.935950539335167));
#3348=CARTESIAN_POINT('Ctrl Pts',(-1.6211138875,5.28125000095592,0.));
#3349=CARTESIAN_POINT('Ctrl Pts',(-1.6211138875,5.22291666762259,-0.935950539335166));
#3350=CARTESIAN_POINT('Ctrl Pts',(-0.81055694375,5.16458333428925,-1.40392580900275));
#3351=CARTESIAN_POINT('Ctrl Pts',(-1.14620883215705E-16,5.10625000095592,
-1.87190107867033));
#3352=CARTESIAN_POINT('Ctrl Pts',(0.81055694375,5.04791666762258,-1.40392580900275));
#3353=CARTESIAN_POINT('Ctrl Pts',(1.6211138875,4.98958333428925,-0.935950539335166));
#3354=CARTESIAN_POINT('Ctrl Pts',(1.6211138875,4.93125000095593,-1.9852919333802E-16));
#3355=CARTESIAN_POINT('Origin',(-2.77555756156289E-16,71.6937500009559,
-2.08166817117217E-16));
#3356=CARTESIAN_POINT('',(1.6211138875,4.05625000095593,-2.08166817117217E-16));
#3357=CARTESIAN_POINT('',(1.6211138875,4.23125000095592,-2.08166817117217E-16));
#3358=CARTESIAN_POINT('',(1.6211138875,71.6937500009559,-2.17804440896414E-16));
#3359=CARTESIAN_POINT('Ctrl Pts',(1.6211138875,4.75625000095593,-1.9852919333802E-16));
#3360=CARTESIAN_POINT('Ctrl Pts',(1.6211138875,4.69791666762259,0.935950539335165));
#3361=CARTESIAN_POINT('Ctrl Pts',(0.810556943750001,4.63958333428927,1.40392580900275));
#3362=CARTESIAN_POINT('Ctrl Pts',(3.43862649647115E-16,4.58125000095593,
1.87190107867033));
#3363=CARTESIAN_POINT('Ctrl Pts',(-0.810556943749999,4.5229166676226,1.40392580900275));
#3364=CARTESIAN_POINT('Ctrl Pts',(-1.6211138875,4.46458333428926,0.935950539335167));
#3365=CARTESIAN_POINT('Ctrl Pts',(-1.6211138875,4.40625000095593,0.));
#3366=CARTESIAN_POINT('Ctrl Pts',(-1.6211138875,4.34791666762259,-0.935950539335166));
#3367=CARTESIAN_POINT('Ctrl Pts',(-0.81055694375,4.28958333428926,-1.40392580900275));
#3368=CARTESIAN_POINT('Ctrl Pts',(-1.14620883215705E-16,4.23125000095592,
-1.87190107867033));
#3369=CARTESIAN_POINT('Ctrl Pts',(0.81055694375,4.17291666762259,-1.40392580900275));
#3370=CARTESIAN_POINT('Ctrl Pts',(1.6211138875,4.11458333428925,-0.935950539335166));
#3371=CARTESIAN_POINT('Ctrl Pts',(1.6211138875,4.05625000095593,-1.9852919333802E-16));
#3372=CARTESIAN_POINT('Ctrl Pts',(1.6211138875,4.93125000095593,-1.9852919333802E-16));
#3373=CARTESIAN_POINT('Ctrl Pts',(1.6211138875,4.87291666762259,0.935950539335165));
#3374=CARTESIAN_POINT('Ctrl Pts',(0.810556943750001,4.81458333428926,1.40392580900275));
#3375=CARTESIAN_POINT('Ctrl Pts',(3.43862649647115E-16,4.75625000095592,
1.87190107867033));
#3376=CARTESIAN_POINT('Ctrl Pts',(-0.810556943749999,4.69791666762259,1.40392580900275));
#3377=CARTESIAN_POINT('Ctrl Pts',(-1.6211138875,4.63958333428925,0.935950539335167));
#3378=CARTESIAN_POINT('Ctrl Pts',(-1.6211138875,4.58125000095593,0.));
#3379=CARTESIAN_POINT('Ctrl Pts',(-1.6211138875,4.52291666762258,-0.935950539335166));
#3380=CARTESIAN_POINT('Ctrl Pts',(-0.81055694375,4.46458333428926,-1.40392580900275));
#3381=CARTESIAN_POINT('Ctrl Pts',(-1.14620883215705E-16,4.40625000095592,
-1.87190107867033));
#3382=CARTESIAN_POINT('Ctrl Pts',(0.81055694375,4.34791666762259,-1.40392580900275));
#3383=CARTESIAN_POINT('Ctrl Pts',(1.6211138875,4.28958333428925,-0.935950539335166));
#3384=CARTESIAN_POINT('Ctrl Pts',(1.6211138875,4.23125000095592,-1.9852919333802E-16));
#3385=CARTESIAN_POINT('Origin',(-2.77555756156289E-16,71.6937500009559,
-2.08166817117217E-16));
#3386=CARTESIAN_POINT('',(1.6211138875,3.35625000095592,-2.08166817117217E-16));
#3387=CARTESIAN_POINT('',(1.6211138875,3.53125000095592,-2.08166817117217E-16));
#3388=CARTESIAN_POINT('',(1.6211138875,71.6937500009559,-2.17804440896414E-16));
#3389=CARTESIAN_POINT('Ctrl Pts',(1.6211138875,4.05625000095593,-1.9852919333802E-16));
#3390=CARTESIAN_POINT('Ctrl Pts',(1.6211138875,3.9979166676226,0.935950539335165));
#3391=CARTESIAN_POINT('Ctrl Pts',(0.810556943750001,3.93958333428926,1.40392580900275));
#3392=CARTESIAN_POINT('Ctrl Pts',(3.43862649647115E-16,3.88125000095593,
1.87190107867033));
#3393=CARTESIAN_POINT('Ctrl Pts',(-0.810556943749999,3.82291666762259,1.40392580900275));
#3394=CARTESIAN_POINT('Ctrl Pts',(-1.6211138875,3.76458333428926,0.935950539335167));
#3395=CARTESIAN_POINT('Ctrl Pts',(-1.6211138875,3.70625000095592,0.));
#3396=CARTESIAN_POINT('Ctrl Pts',(-1.6211138875,3.6479166676226,-0.935950539335166));
#3397=CARTESIAN_POINT('Ctrl Pts',(-0.81055694375,3.58958333428926,-1.40392580900275));
#3398=CARTESIAN_POINT('Ctrl Pts',(-1.14620883215705E-16,3.53125000095593,
-1.87190107867033));
#3399=CARTESIAN_POINT('Ctrl Pts',(0.81055694375,3.47291666762259,-1.40392580900275));
#3400=CARTESIAN_POINT('Ctrl Pts',(1.6211138875,3.41458333428926,-0.935950539335166));
#3401=CARTESIAN_POINT('Ctrl Pts',(1.6211138875,3.35625000095592,-1.9852919333802E-16));
#3402=CARTESIAN_POINT('Ctrl Pts',(1.6211138875,4.23125000095592,-1.9852919333802E-16));
#3403=CARTESIAN_POINT('Ctrl Pts',(1.6211138875,4.17291666762259,0.935950539335165));
#3404=CARTESIAN_POINT('Ctrl Pts',(0.810556943750001,4.11458333428925,1.40392580900275));
#3405=CARTESIAN_POINT('Ctrl Pts',(3.43862649647115E-16,4.05625000095593,
1.87190107867033));
#3406=CARTESIAN_POINT('Ctrl Pts',(-0.810556943749999,3.99791666762259,1.40392580900275));
#3407=CARTESIAN_POINT('Ctrl Pts',(-1.6211138875,3.93958333428926,0.935950539335167));
#3408=CARTESIAN_POINT('Ctrl Pts',(-1.6211138875,3.88125000095592,0.));
#3409=CARTESIAN_POINT('Ctrl Pts',(-1.6211138875,3.82291666762259,-0.935950539335166));
#3410=CARTESIAN_POINT('Ctrl Pts',(-0.81055694375,3.76458333428925,-1.40392580900275));
#3411=CARTESIAN_POINT('Ctrl Pts',(-1.14620883215705E-16,3.70625000095592,
-1.87190107867033));
#3412=CARTESIAN_POINT('Ctrl Pts',(0.81055694375,3.64791666762258,-1.40392580900275));
#3413=CARTESIAN_POINT('Ctrl Pts',(1.6211138875,3.58958333428926,-0.935950539335166));
#3414=CARTESIAN_POINT('Ctrl Pts',(1.6211138875,3.53125000095592,-1.9852919333802E-16));
#3415=CARTESIAN_POINT('Origin',(-2.77555756156289E-16,71.6937500009559,
-2.08166817117217E-16));
#3416=CARTESIAN_POINT('',(1.6211138875,2.65625000095593,-2.08166817117217E-16));
#3417=CARTESIAN_POINT('',(1.6211138875,2.83125000095592,-2.08166817117217E-16));
#3418=CARTESIAN_POINT('',(1.6211138875,71.6937500009559,-2.17804440896414E-16));
#3419=CARTESIAN_POINT('Ctrl Pts',(1.6211138875,3.35625000095592,-1.9852919333802E-16));
#3420=CARTESIAN_POINT('Ctrl Pts',(1.6211138875,3.29791666762259,0.935950539335165));
#3421=CARTESIAN_POINT('Ctrl Pts',(0.810556943750001,3.23958333428925,1.40392580900275));
#3422=CARTESIAN_POINT('Ctrl Pts',(3.43862649647115E-16,3.18125000095593,
1.87190107867033));
#3423=CARTESIAN_POINT('Ctrl Pts',(-0.810556943749999,3.1229166676226,1.40392580900275));
#3424=CARTESIAN_POINT('Ctrl Pts',(-1.6211138875,3.06458333428926,0.935950539335167));
#3425=CARTESIAN_POINT('Ctrl Pts',(-1.6211138875,3.00625000095593,0.));
#3426=CARTESIAN_POINT('Ctrl Pts',(-1.6211138875,2.94791666762259,-0.935950539335166));
#3427=CARTESIAN_POINT('Ctrl Pts',(-0.81055694375,2.88958333428926,-1.40392580900275));
#3428=CARTESIAN_POINT('Ctrl Pts',(-1.14620883215705E-16,2.83125000095592,
-1.87190107867033));
#3429=CARTESIAN_POINT('Ctrl Pts',(0.81055694375,2.7729166676226,-1.40392580900275));
#3430=CARTESIAN_POINT('Ctrl Pts',(1.6211138875,2.71458333428926,-0.935950539335166));
#3431=CARTESIAN_POINT('Ctrl Pts',(1.6211138875,2.65625000095593,-1.9852919333802E-16));
#3432=CARTESIAN_POINT('Ctrl Pts',(1.6211138875,3.53125000095592,-1.9852919333802E-16));
#3433=CARTESIAN_POINT('Ctrl Pts',(1.6211138875,3.47291666762259,0.935950539335165));
#3434=CARTESIAN_POINT('Ctrl Pts',(0.810556943750001,3.41458333428925,1.40392580900275));
#3435=CARTESIAN_POINT('Ctrl Pts',(3.43862649647115E-16,3.35625000095592,
1.87190107867033));
#3436=CARTESIAN_POINT('Ctrl Pts',(-0.810556943749999,3.29791666762259,1.40392580900275));
#3437=CARTESIAN_POINT('Ctrl Pts',(-1.6211138875,3.23958333428925,0.935950539335167));
#3438=CARTESIAN_POINT('Ctrl Pts',(-1.6211138875,3.18125000095593,0.));
#3439=CARTESIAN_POINT('Ctrl Pts',(-1.6211138875,3.12291666762259,-0.935950539335166));
#3440=CARTESIAN_POINT('Ctrl Pts',(-0.81055694375,3.06458333428926,-1.40392580900275));
#3441=CARTESIAN_POINT('Ctrl Pts',(-1.14620883215705E-16,3.00625000095592,
-1.87190107867033));
#3442=CARTESIAN_POINT('Ctrl Pts',(0.81055694375,2.94791666762259,-1.40392580900275));
#3443=CARTESIAN_POINT('Ctrl Pts',(1.6211138875,2.88958333428925,-0.935950539335166));
#3444=CARTESIAN_POINT('Ctrl Pts',(1.6211138875,2.83125000095592,-1.9852919333802E-16));
#3445=CARTESIAN_POINT('Origin',(-2.77555756156289E-16,71.6937500009559,
-2.08166817117217E-16));
#3446=CARTESIAN_POINT('',(1.6211138875,1.95625000095592,-2.08166817117217E-16));
#3447=CARTESIAN_POINT('',(1.6211138875,2.13125000095592,-2.08166817117217E-16));
#3448=CARTESIAN_POINT('',(1.6211138875,71.6937500009559,-2.17804440896414E-16));
#3449=CARTESIAN_POINT('Ctrl Pts',(1.6211138875,2.65625000095593,-1.9852919333802E-16));
#3450=CARTESIAN_POINT('Ctrl Pts',(1.6211138875,2.59791666762259,0.935950539335165));
#3451=CARTESIAN_POINT('Ctrl Pts',(0.810556943750001,2.53958333428926,1.40392580900275));
#3452=CARTESIAN_POINT('Ctrl Pts',(3.43862649647115E-16,2.48125000095592,
1.87190107867033));
#3453=CARTESIAN_POINT('Ctrl Pts',(-0.810556943749999,2.42291666762259,1.40392580900275));
#3454=CARTESIAN_POINT('Ctrl Pts',(-1.6211138875,2.36458333428927,0.935950539335167));
#3455=CARTESIAN_POINT('Ctrl Pts',(-1.6211138875,2.30625000095593,0.));
#3456=CARTESIAN_POINT('Ctrl Pts',(-1.6211138875,2.2479166676226,-0.935950539335166));
#3457=CARTESIAN_POINT('Ctrl Pts',(-0.81055694375,2.18958333428926,-1.40392580900275));
#3458=CARTESIAN_POINT('Ctrl Pts',(-1.14620883215705E-16,2.13125000095593,
-1.87190107867033));
#3459=CARTESIAN_POINT('Ctrl Pts',(0.81055694375,2.07291666762259,-1.40392580900275));
#3460=CARTESIAN_POINT('Ctrl Pts',(1.6211138875,2.01458333428926,-0.935950539335166));
#3461=CARTESIAN_POINT('Ctrl Pts',(1.6211138875,1.95625000095592,-1.9852919333802E-16));
#3462=CARTESIAN_POINT('Ctrl Pts',(1.6211138875,2.83125000095592,-1.9852919333802E-16));
#3463=CARTESIAN_POINT('Ctrl Pts',(1.6211138875,2.77291666762258,0.935950539335165));
#3464=CARTESIAN_POINT('Ctrl Pts',(0.810556943750001,2.71458333428926,1.40392580900275));
#3465=CARTESIAN_POINT('Ctrl Pts',(3.43862649647115E-16,2.65625000095591,
1.87190107867033));
#3466=CARTESIAN_POINT('Ctrl Pts',(-0.810556943749999,2.59791666762259,1.40392580900275));
#3467=CARTESIAN_POINT('Ctrl Pts',(-1.6211138875,2.53958333428926,0.935950539335167));
#3468=CARTESIAN_POINT('Ctrl Pts',(-1.6211138875,2.48125000095592,0.));
#3469=CARTESIAN_POINT('Ctrl Pts',(-1.6211138875,2.42291666762259,-0.935950539335166));
#3470=CARTESIAN_POINT('Ctrl Pts',(-0.81055694375,2.36458333428925,-1.40392580900275));
#3471=CARTESIAN_POINT('Ctrl Pts',(-1.14620883215705E-16,2.30625000095593,
-1.87190107867033));
#3472=CARTESIAN_POINT('Ctrl Pts',(0.81055694375,2.24791666762258,-1.40392580900275));
#3473=CARTESIAN_POINT('Ctrl Pts',(1.6211138875,2.18958333428926,-0.935950539335166));
#3474=CARTESIAN_POINT('Ctrl Pts',(1.6211138875,2.13125000095592,-1.9852919333802E-16));
#3475=CARTESIAN_POINT('Origin',(-2.77555756156289E-16,71.6937500009559,
-2.08166817117217E-16));
#3476=CARTESIAN_POINT('',(1.6211138875,1.25625000095593,-2.08166817117217E-16));
#3477=CARTESIAN_POINT('',(1.6211138875,1.43125000095592,-2.08166817117217E-16));
#3478=CARTESIAN_POINT('',(1.6211138875,71.6937500009559,-2.17804440896414E-16));
#3479=CARTESIAN_POINT('Ctrl Pts',(1.6211138875,1.95625000095592,-1.9852919333802E-16));
#3480=CARTESIAN_POINT('Ctrl Pts',(1.6211138875,1.8979166676226,0.935950539335165));
#3481=CARTESIAN_POINT('Ctrl Pts',(0.810556943750001,1.83958333428925,1.40392580900275));
#3482=CARTESIAN_POINT('Ctrl Pts',(3.43862649647115E-16,1.78125000095593,
1.87190107867033));
#3483=CARTESIAN_POINT('Ctrl Pts',(-0.810556943749999,1.72291666762259,1.40392580900275));
#3484=CARTESIAN_POINT('Ctrl Pts',(-1.6211138875,1.66458333428926,0.935950539335167));
#3485=CARTESIAN_POINT('Ctrl Pts',(-1.6211138875,1.60625000095593,0.));
#3486=CARTESIAN_POINT('Ctrl Pts',(-1.6211138875,1.54791666762259,-0.935950539335166));
#3487=CARTESIAN_POINT('Ctrl Pts',(-0.81055694375,1.48958333428927,-1.40392580900275));
#3488=CARTESIAN_POINT('Ctrl Pts',(-1.14620883215705E-16,1.43125000095592,
-1.87190107867033));
#3489=CARTESIAN_POINT('Ctrl Pts',(0.81055694375,1.3729166676226,-1.40392580900275));
#3490=CARTESIAN_POINT('Ctrl Pts',(1.6211138875,1.31458333428926,-0.935950539335166));
#3491=CARTESIAN_POINT('Ctrl Pts',(1.6211138875,1.25625000095593,-1.9852919333802E-16));
#3492=CARTESIAN_POINT('Ctrl Pts',(1.6211138875,2.13125000095592,-1.9852919333802E-16));
#3493=CARTESIAN_POINT('Ctrl Pts',(1.6211138875,2.07291666762259,0.935950539335165));
#3494=CARTESIAN_POINT('Ctrl Pts',(0.810556943750001,2.01458333428925,1.40392580900275));
#3495=CARTESIAN_POINT('Ctrl Pts',(3.43862649647115E-16,1.95625000095592,
1.87190107867033));
#3496=CARTESIAN_POINT('Ctrl Pts',(-0.810556943749999,1.89791666762258,1.40392580900275));
#3497=CARTESIAN_POINT('Ctrl Pts',(-1.6211138875,1.83958333428925,0.935950539335167));
#3498=CARTESIAN_POINT('Ctrl Pts',(-1.6211138875,1.78125000095593,0.));
#3499=CARTESIAN_POINT('Ctrl Pts',(-1.6211138875,1.72291666762259,-0.935950539335166));
#3500=CARTESIAN_POINT('Ctrl Pts',(-0.81055694375,1.66458333428926,-1.40392580900275));
#3501=CARTESIAN_POINT('Ctrl Pts',(-1.14620883215705E-16,1.60625000095592,
-1.87190107867033));
#3502=CARTESIAN_POINT('Ctrl Pts',(0.81055694375,1.54791666762259,-1.40392580900275));
#3503=CARTESIAN_POINT('Ctrl Pts',(1.6211138875,1.48958333428925,-0.935950539335166));
#3504=CARTESIAN_POINT('Ctrl Pts',(1.6211138875,1.43125000095592,-1.9852919333802E-16));
#3505=CARTESIAN_POINT('Origin',(-2.77555756156289E-16,71.6937500009559,
-2.08166817117217E-16));
#3506=CARTESIAN_POINT('',(1.6211138875,0.556250000955924,-2.08166817117217E-16));
#3507=CARTESIAN_POINT('',(1.6211138875,0.731250000955919,-2.08166817117217E-16));
#3508=CARTESIAN_POINT('',(1.6211138875,71.6937500009559,-2.17804440896414E-16));
#3509=CARTESIAN_POINT('Ctrl Pts',(1.6211138875,1.25625000095593,-1.9852919333802E-16));
#3510=CARTESIAN_POINT('Ctrl Pts',(1.6211138875,1.19791666762259,0.935950539335165));
#3511=CARTESIAN_POINT('Ctrl Pts',(0.810556943750001,1.13958333428926,1.40392580900275));
#3512=CARTESIAN_POINT('Ctrl Pts',(3.43862649647115E-16,1.08125000095592,
1.87190107867033));
#3513=CARTESIAN_POINT('Ctrl Pts',(-0.810556943749999,1.02291666762259,1.40392580900275));
#3514=CARTESIAN_POINT('Ctrl Pts',(-1.6211138875,0.964583334289254,0.935950539335167));
#3515=CARTESIAN_POINT('Ctrl Pts',(-1.6211138875,0.906250000955927,0.));
#3516=CARTESIAN_POINT('Ctrl Pts',(-1.6211138875,0.8479166676226,-0.935950539335166));
#3517=CARTESIAN_POINT('Ctrl Pts',(-0.81055694375,0.789583334289259,-1.40392580900275));
#3518=CARTESIAN_POINT('Ctrl Pts',(-1.14620883215705E-16,0.731250000955933,
-1.87190107867033));
#3519=CARTESIAN_POINT('Ctrl Pts',(0.81055694375,0.672916667622592,-1.40392580900275));
#3520=CARTESIAN_POINT('Ctrl Pts',(1.6211138875,0.614583334289265,-0.935950539335166));
#3521=CARTESIAN_POINT('Ctrl Pts',(1.6211138875,0.556250000955924,-1.9852919333802E-16));
#3522=CARTESIAN_POINT('Ctrl Pts',(1.6211138875,1.43125000095592,-1.9852919333802E-16));
#3523=CARTESIAN_POINT('Ctrl Pts',(1.6211138875,1.37291666762258,0.935950539335165));
#3524=CARTESIAN_POINT('Ctrl Pts',(0.810556943750001,1.31458333428926,1.40392580900275));
#3525=CARTESIAN_POINT('Ctrl Pts',(3.43862649647115E-16,1.25625000095592,
1.87190107867033));
#3526=CARTESIAN_POINT('Ctrl Pts',(-0.810556943749999,1.19791666762259,1.40392580900275));
#3527=CARTESIAN_POINT('Ctrl Pts',(-1.6211138875,1.13958333428925,0.935950539335167));
#3528=CARTESIAN_POINT('Ctrl Pts',(-1.6211138875,1.08125000095592,0.));
#3529=CARTESIAN_POINT('Ctrl Pts',(-1.6211138875,1.02291666762259,-0.935950539335166));
#3530=CARTESIAN_POINT('Ctrl Pts',(-0.81055694375,0.964583334289254,-1.40392580900275));
#3531=CARTESIAN_POINT('Ctrl Pts',(-1.14620883215705E-16,0.906250000955927,
-1.87190107867033));
#3532=CARTESIAN_POINT('Ctrl Pts',(0.81055694375,0.847916667622586,-1.40392580900275));
#3533=CARTESIAN_POINT('Ctrl Pts',(1.6211138875,0.789583334289259,-0.935950539335166));
#3534=CARTESIAN_POINT('Ctrl Pts',(1.6211138875,0.731250000955919,-1.9852919333802E-16));
#3535=CARTESIAN_POINT('Origin',(0.,70.,0.));
#3536=CARTESIAN_POINT('',(9.45320890747724E-15,9.17500000000001,2.));
#3537=CARTESIAN_POINT('',(1.59948180381188E-6,9.26250009520725,1.9999999999842));
#3538=CARTESIAN_POINT('',(-2.44929359829471E-16,70.,2.));
#3539=CARTESIAN_POINT('',(0.0859174328513604,9.52000000000001,-1.99815344810835));
#3540=CARTESIAN_POINT('Ctrl Pts',(7.0652298666267E-16,9.17500000000001,
2.));
#3541=CARTESIAN_POINT('Ctrl Pts',(0.0654772424788999,9.17881950581128,2.));
#3542=CARTESIAN_POINT('Ctrl Pts',(0.131032570471315,9.18264356661088,1.99678463284646));
#3543=CARTESIAN_POINT('Ctrl Pts',(0.450361646577216,9.20127109605039,1.96526945131892));
#3544=CARTESIAN_POINT('Ctrl Pts',(0.697209761447221,9.2156705694178,1.89183809047694));
#3545=CARTESIAN_POINT('Ctrl Pts',(1.1599092090385,9.2426613705273,1.65093392830596));
#3546=CARTESIAN_POINT('Ctrl Pts',(1.36930582965127,9.25674167404953,1.48190465126004));
#3547=CARTESIAN_POINT('Ctrl Pts',(1.7065994308231,9.28712492813149,1.07520874818695));
#3548=CARTESIAN_POINT('Ctrl Pts',(1.83255618803444,9.30253994528419,0.842791711206109));
#3549=CARTESIAN_POINT('Ctrl Pts',(1.9852210179839,9.33184741278064,0.35079538907281));
#3550=CARTESIAN_POINT('Ctrl Pts',(2.01363857356743,9.3447081787264,0.0968766608571719));
#3551=CARTESIAN_POINT('Ctrl Pts',(1.97330694803748,9.3719962043763,-0.420000685587666));
#3552=CARTESIAN_POINT('Ctrl Pts',(1.90028788275951,9.38714172438564,-0.677646653316077));
#3553=CARTESIAN_POINT('Ctrl Pts',(1.66096748133944,9.41766878114948,-1.14375396451092));
#3554=CARTESIAN_POINT('Ctrl Pts',(1.4991644205791,9.43275134166329,-1.34889419374688));
#3555=CARTESIAN_POINT('Ctrl Pts',(1.13680344977255,9.4590353597047,-1.65997361456257));
#3556=CARTESIAN_POINT('Ctrl Pts',(0.948658523269392,9.46966158614263,-1.77422571002165));
#3557=CARTESIAN_POINT('Ctrl Pts',(0.535425634758868,9.49376683797241,-1.94028063464073));
#3558=CARTESIAN_POINT('Ctrl Pts',(0.312304096132736,9.50678226105893,-1.98841950664599));
#3559=CARTESIAN_POINT('Ctrl Pts',(0.0859167558215111,9.51998818924375,-1.99815372558498));
#3560=CARTESIAN_POINT('',(-2.44929359829471E-16,9.52000000000001,2.));
#3561=CARTESIAN_POINT('Origin',(0.,9.52000000000001,0.));
#3562=CARTESIAN_POINT('',(2.44929359829471E-16,9.65431457505077,2.));
#3563=CARTESIAN_POINT('',(-2.44929359829471E-16,70.,2.));
#3564=CARTESIAN_POINT('',(-2.44929359829471E-16,9.65431457505077,-2.));
#3565=CARTESIAN_POINT('Origin',(0.,9.65431457505077,0.));
#3566=CARTESIAN_POINT('Origin',(0.,9.65431457505077,0.));
#3567=CARTESIAN_POINT('',(1.48658736561886,9.52000000000002,-1.33792828622799));
#3568=CARTESIAN_POINT('Origin',(0.,9.52000000000001,0.));
#3569=CARTESIAN_POINT('Ctrl Pts',(1.48734101297985,9.52000000000002,-1.33709263370496));
#3570=CARTESIAN_POINT('Ctrl Pts',(1.63791501835166,9.50714677517763,-1.169598708428));
#3571=CARTESIAN_POINT('Ctrl Pts',(1.75911955738823,9.49392572967888,-0.977867352719137));
#3572=CARTESIAN_POINT('Ctrl Pts',(1.93092564010499,9.46810888677228,-0.566018685335447));
#3573=CARTESIAN_POINT('Ctrl Pts',(1.98163283227066,9.45568175477737,-0.349301079153031));
#3574=CARTESIAN_POINT('Ctrl Pts',(2.01214704636104,9.43088073657671,0.124014372304799));
#3575=CARTESIAN_POINT('Ctrl Pts',(1.98031191750013,9.41785399914761,0.37752308269164));
#3576=CARTESIAN_POINT('Ctrl Pts',(1.82071231212849,9.3884011807903,0.868392811035422));
#3577=CARTESIAN_POINT('Ctrl Pts',(1.69094028902841,9.372919972832,1.09991733862416));
#3578=CARTESIAN_POINT('Ctrl Pts',(1.35539802709022,9.34330775640548,1.49236179051775));
#3579=CARTESIAN_POINT('Ctrl Pts',(1.15560569732876,9.32991033425602,1.65189509908556));
#3580=CARTESIAN_POINT('Ctrl Pts',(0.790412681009631,9.30860740830407,1.84408113448345));
#3581=CARTESIAN_POINT('Ctrl Pts',(0.641067231556676,9.29989559041931,1.90115935094908));
#3582=CARTESIAN_POINT('Ctrl Pts',(0.327456843583413,9.28160165112087,1.97981779131892));
#3583=CARTESIAN_POINT('Ctrl Pts',(0.164054865481099,9.2720698690649,1.99999671982436));
#3584=CARTESIAN_POINT('Ctrl Pts',(3.99936387195099E-5,9.2625023348741,1.99999999960013));
#3585=CARTESIAN_POINT('Origin',(0.,70.,0.));
#3586=CARTESIAN_POINT('',(-8.37541161687439E-15,8.475,2.));
#3587=CARTESIAN_POINT('',(1.48308516830053E-14,8.56250000191184,2.));
#3588=CARTESIAN_POINT('',(-2.44929359829471E-16,70.,2.));
#3589=CARTESIAN_POINT('Ctrl Pts',(7.59808882477842E-15,8.47500000000001,
2.));
#3590=CARTESIAN_POINT('Ctrl Pts',(0.105462367466573,8.48115197143556,2.));
#3591=CARTESIAN_POINT('Ctrl Pts',(0.211002460351238,8.48730847685385,1.99165844030807));
#3592=CARTESIAN_POINT('Ctrl Pts',(0.566317225824197,8.50803517150644,1.93487381835091));
#3593=CARTESIAN_POINT('Ctrl Pts',(0.807005156353637,8.52187416873751,1.84745781454963));
#3594=CARTESIAN_POINT('Ctrl Pts',(1.25252964810262,8.54829920549905,1.58160142821606));
#3595=CARTESIAN_POINT('Ctrl Pts',(1.4508881784191,8.56316568976568,1.40184370960763));
#3596=CARTESIAN_POINT('Ctrl Pts',(1.7631873502528,8.59362166091542,0.979277841388434));
#3597=CARTESIAN_POINT('Ctrl Pts',(1.87558951753305,8.60890636078586,0.741614671450395));
#3598=CARTESIAN_POINT('Ctrl Pts',(2.00138276505221,8.63777309815185,0.242828228006081));
#3599=CARTESIAN_POINT('Ctrl Pts',(2.01601583216441,8.65018696662936,-0.012947724454868));
#3600=CARTESIAN_POINT('Ctrl Pts',(1.94699225367654,8.67831894957769,-0.529965786082098));
#3601=CARTESIAN_POINT('Ctrl Pts',(1.85867649225116,8.69380137912261,-0.785449281408499));
#3602=CARTESIAN_POINT('Ctrl Pts',(1.59200912501479,8.7244228066855,-1.23763587188446));
#3603=CARTESIAN_POINT('Ctrl Pts',(1.41968985468868,8.73926989008554,-1.43204332669598));
#3604=CARTESIAN_POINT('Ctrl Pts',(1.00937069646563,8.76709572606385,-1.74595415512816));
#3605=CARTESIAN_POINT('Ctrl Pts',(0.774881221579688,8.77979859540789,-1.86192286742975));
#3606=CARTESIAN_POINT('Ctrl Pts',(0.269671873081754,8.80926914073694,-1.99928612004507));
#3607=CARTESIAN_POINT('Ctrl Pts',(0.00338211962886355,8.82480270968836,
-2.01738559898112));
#3608=CARTESIAN_POINT('Ctrl Pts',(-0.510960934847595,8.85480605453282,-1.95029153797676));
#3609=CARTESIAN_POINT('Ctrl Pts',(-0.754687604120902,8.86902344357376,-1.86954848788297));
#3610=CARTESIAN_POINT('Ctrl Pts',(-1.20800875702901,8.8954671774934,-1.61584007525765));
#3611=CARTESIAN_POINT('Ctrl Pts',(-1.41133074637823,8.90999891019387,-1.44169119402485));
#3612=CARTESIAN_POINT('Ctrl Pts',(-1.73576755166978,8.94039724159011,-1.02727396296809));
#3613=CARTESIAN_POINT('Ctrl Pts',(-1.85492262965682,8.95575220708085,-0.792118689280096));
#3614=CARTESIAN_POINT('Ctrl Pts',(-1.99405667036303,8.98484046001804,-0.296649685242302));
#3615=CARTESIAN_POINT('Ctrl Pts',(-2.01556246576001,8.99743240884776,-0.0418401299621862));
#3616=CARTESIAN_POINT('Ctrl Pts',(-1.96104169758539,9.02508165764329,0.473995475055345));
#3617=CARTESIAN_POINT('Ctrl Pts',(-1.88096840075696,9.04032842551777,0.729572868260019));
#3618=CARTESIAN_POINT('Ctrl Pts',(-1.62924249842628,9.07084754148429,1.18836067314294));
#3619=CARTESIAN_POINT('Ctrl Pts',(-1.46241462989662,9.08582531086932,1.38852550186937));
#3620=CARTESIAN_POINT('Ctrl Pts',(-1.06248382247422,9.11392601041099,1.71387493493997));
#3621=CARTESIAN_POINT('Ctrl Pts',(-0.833398741972677,9.12638507338498,1.83621648971916));
#3622=CARTESIAN_POINT('Ctrl Pts',(-0.396706359840074,9.15185879567604,1.97038257217702));
#3623=CARTESIAN_POINT('Ctrl Pts',(-0.198712772962524,9.16340842157719,2.));
#3624=CARTESIAN_POINT('Ctrl Pts',(-8.53483950180589E-15,9.17500000000001,
2.));
#3625=CARTESIAN_POINT('Ctrl Pts',(1.90566659674651E-11,9.26250000191294,
2.00000000000002));
#3626=CARTESIAN_POINT('Ctrl Pts',(-0.257304108099317,9.24749059560743,2.00000000000006));
#3627=CARTESIAN_POINT('Ctrl Pts',(-0.512236880529356,9.23261951721429,1.95034594378667));
#3628=CARTESIAN_POINT('Ctrl Pts',(-0.981276227019413,9.20525888866904,1.76038092822654));
#3629=CARTESIAN_POINT('Ctrl Pts',(-1.19231374107119,9.19314353837047,1.62488180827426));
#3630=CARTESIAN_POINT('Ctrl Pts',(-1.5622316908883,9.16470757636485,1.27556796811243));
#3631=CARTESIAN_POINT('Ctrl Pts',(-1.71468144646498,9.14946372091359,1.06183479387747));
#3632=CARTESIAN_POINT('Ctrl Pts',(-1.93127233317037,9.11898066356148,0.583475553719287));
#3633=CARTESIAN_POINT('Ctrl Pts',(-1.99153619176926,9.10404547537348,0.322628854278394));
#3634=CARTESIAN_POINT('Ctrl Pts',(-2.00646871390316,9.07742145493661,-0.19576877688697));
#3635=CARTESIAN_POINT('Ctrl Pts',(-1.96554314136245,9.06384851194789,-0.448284406729788));
#3636=CARTESIAN_POINT('Ctrl Pts',(-1.78817028005374,9.03415566366629,-0.933644101450979));
#3637=CARTESIAN_POINT('Ctrl Pts',(-1.64995028952709,9.01866059682148,-1.16056553033455));
#3638=CARTESIAN_POINT('Ctrl Pts',(-1.29415730903856,8.98874903328475,-1.54724376046733));
#3639=CARTESIAN_POINT('Ctrl Pts',(-1.08034993983026,8.97552041506857,-1.70341423900341));
#3640=CARTESIAN_POINT('Ctrl Pts',(-0.609968446726665,8.94808149463753,-1.92189375954845));
#3641=CARTESIAN_POINT('Ctrl Pts',(-0.358856680588314,8.93343330827946,-1.98416774025015));
#3642=CARTESIAN_POINT('Ctrl Pts',(0.163198666704829,8.90298007968736,-2.0110569238483));
#3643=CARTESIAN_POINT('Ctrl Pts',(0.42937403919576,8.88745318295873,-1.97145826744264));
#3644=CARTESIAN_POINT('Ctrl Pts',(0.92000150326077,8.85883324755494,-1.79408447591622));
#3645=CARTESIAN_POINT('Ctrl Pts',(1.14116649734624,8.84652018704735,-1.66219224268598));
#3646=CARTESIAN_POINT('Ctrl Pts',(1.5251146797244,8.81801352796414,-1.3195793218663));
#3647=CARTESIAN_POINT('Ctrl Pts',(1.68318697174025,8.80286160175781,-1.1109120476771));
#3648=CARTESIAN_POINT('Ctrl Pts',(1.91338699615764,8.77234334845276,-0.639713347655176));
#3649=CARTESIAN_POINT('Ctrl Pts',(1.98126220145905,8.75727847929295,-0.380694043773767));
#3650=CARTESIAN_POINT('Ctrl Pts',(2.01131636650622,8.7302565099176,0.136850448845239));
#3651=CARTESIAN_POINT('Ctrl Pts',(1.97786148928562,8.71714353473363,0.390171872482263));
#3652=CARTESIAN_POINT('Ctrl Pts',(1.81527538666286,8.68767894754209,0.879550308535442));
#3653=CARTESIAN_POINT('Ctrl Pts',(1.68436773280673,8.67222716163985,1.10983677648947));
#3654=CARTESIAN_POINT('Ctrl Pts',(1.33956700707109,8.64202942504695,1.50852614526927));
#3655=CARTESIAN_POINT('Ctrl Pts',(1.12839208065064,8.62832287328311,1.67235528110575));
#3656=CARTESIAN_POINT('Ctrl Pts',(0.662588073022141,8.60115097283811,1.90430099781709));
#3657=CARTESIAN_POINT('Ctrl Pts',(0.413980559775339,8.58664886789871,1.97331305372972));
#3658=CARTESIAN_POINT('Ctrl Pts',(0.106132978563006,8.56869109232799,1.99789044226144));
#3659=CARTESIAN_POINT('Ctrl Pts',(0.0530358871513877,8.56559376199567,2.));
#3660=CARTESIAN_POINT('Ctrl Pts',(7.41933818794109E-16,8.56250000191184,
2.));
#3661=CARTESIAN_POINT('Origin',(0.,70.,0.));
#3662=CARTESIAN_POINT('',(1.33173054502156E-14,7.77500000000001,2.));
#3663=CARTESIAN_POINT('',(2.75550483792952E-14,7.86250000191184,2.));
#3664=CARTESIAN_POINT('',(-2.44929359829471E-16,70.,2.));
#3665=CARTESIAN_POINT('Ctrl Pts',(5.86336534880161E-15,7.77500000000001,
2.));
#3666=CARTESIAN_POINT('Ctrl Pts',(0.144710179754815,7.78344142715237,2.));
#3667=CARTESIAN_POINT('Ctrl Pts',(0.289338759461054,7.79187809430192,1.98429396284856));
#3668=CARTESIAN_POINT('Ctrl Pts',(0.678641071003376,7.81458739580856,1.89831552691932));
#3669=CARTESIAN_POINT('Ctrl Pts',(0.913286535675115,7.827511604482,1.79722711026655));
#3670=CARTESIAN_POINT('Ctrl Pts',(1.34230244411645,7.8547280067094,1.50617451526789));
#3671=CARTESIAN_POINT('Ctrl Pts',(1.52994621267493,7.86985230922693,1.31512714824939));
#3672=CARTESIAN_POINT('Ctrl Pts',(1.81638341917427,7.90037819173438,0.876245981398777));
#3673=CARTESIAN_POINT('Ctrl Pts',(1.91447157603324,7.91548006520074,0.633937637928994));
#3674=CARTESIAN_POINT('Ctrl Pts',(2.01219327080911,7.943863981205,0.128501460288878));
#3675=CARTESIAN_POINT('Ctrl Pts',(2.01212313264796,7.95619331976415,-0.12959523102893));
#3676=CARTESIAN_POINT('Ctrl Pts',(1.91277780465302,7.98497332866613,-0.641934609574077));
#3677=CARTESIAN_POINT('Ctrl Pts',(1.81050911014114,8.00050874900382,-0.890411320888694));
#3678=CARTESIAN_POINT('Ctrl Pts',(1.5203852399451,8.03089334619851,-1.3243672675752));
#3679=CARTESIAN_POINT('Ctrl Pts',(1.33856236024206,8.04546904366245,-1.5079157626145));
#3680=CARTESIAN_POINT('Ctrl Pts',(0.909424776687682,8.07277395533603,-1.80065014111363));
#3681=CARTESIAN_POINT('Ctrl Pts',(0.66460770222988,8.08623121736996,-1.90466015281606));
#3682=CARTESIAN_POINT('Ctrl Pts',(0.149343889657557,8.11628827310334,-2.01164976474229));
#3683=CARTESIAN_POINT('Ctrl Pts',(-0.11594189746457,8.13176327735213,-2.01385064625415));
#3684=CARTESIAN_POINT('Ctrl Pts',(-0.623007461315161,8.16134210191008,-1.91731213129782));
#3685=CARTESIAN_POINT('Ctrl Pts',(-0.86061755342047,8.17467105579428,-1.8230469408812));
#3686=CARTESIAN_POINT('Ctrl Pts',(-1.29795031623099,8.2014956207513,-1.54455245039818));
#3687=CARTESIAN_POINT('Ctrl Pts',(-1.49103788648041,8.21649747918302,-1.35907182806801));
#3688=CARTESIAN_POINT('Ctrl Pts',(-1.79052008750211,8.24700149799274,-0.928154981291581));
#3689=CARTESIAN_POINT('Ctrl Pts',(-1.89578969583597,8.26220076216339,-0.688065014786461));
#3690=CARTESIAN_POINT('Ctrl Pts',(-2.00756828407403,8.29082923214331,-0.185903675101916));
#3691=CARTESIAN_POINT('Ctrl Pts',(-2.01490631812433,8.30315113975425,0.0709825571365514));
#3692=CARTESIAN_POINT('Ctrl Pts',(-1.93082980082602,8.33160909865332,0.585762450874943));
#3693=CARTESIAN_POINT('Ctrl Pts',(-1.83553236798457,8.3471242386706,0.837862575759251));
#3694=CARTESIAN_POINT('Ctrl Pts',(-1.55708628702896,8.37763996900972,1.28115646027813));
#3695=CARTESIAN_POINT('Ctrl Pts',(-1.37997141252304,8.39235776994509,1.47023604261329));
#3696=CARTESIAN_POINT('Ctrl Pts',(-0.960303803133177,8.41992859304112,1.7737015943198));
#3697=CARTESIAN_POINT('Ctrl Pts',(-0.720770852159437,8.43295503362406,1.88380283908764));
#3698=CARTESIAN_POINT('Ctrl Pts',(-0.313547604702796,8.45670972305903,1.98154568112522));
#3699=CARTESIAN_POINT('Ctrl Pts',(-0.15685977517984,8.46584984644785,2.));
#3700=CARTESIAN_POINT('Ctrl Pts',(2.04697370165263E-14,8.47500000000001,
2.));
#3701=CARTESIAN_POINT('Ctrl Pts',(-6.34908792207511E-15,8.56250000191184,
2.));
#3702=CARTESIAN_POINT('Ctrl Pts',(-0.211791443364041,8.55014550104893,2.));
#3703=CARTESIAN_POINT('Ctrl Pts',(-0.422606866547989,8.53784793469652,1.9663553689863));
#3704=CARTESIAN_POINT('Ctrl Pts',(-0.868081090589095,8.51186193829412,1.81994308052866));
#3705=CARTESIAN_POINT('Ctrl Pts',(-1.09398569432927,8.49949294438145,1.69379772754904));
#3706=CARTESIAN_POINT('Ctrl Pts',(-1.48760806966432,8.4712296434194,1.36158744612626));
#3707=CARTESIAN_POINT('Ctrl Pts',(-1.65102289478909,8.45617923347963,1.15801418579668));
#3708=CARTESIAN_POINT('Ctrl Pts',(-1.89430688679977,8.42565217494147,0.694195219573794));
#3709=CARTESIAN_POINT('Ctrl Pts',(-1.96957247437605,8.41047322719565,0.437184584522383));
#3710=CARTESIAN_POINT('Ctrl Pts',(-2.01441005981556,8.38306971268874,-0.0793773312476014));
#3711=CARTESIAN_POINT('Ctrl Pts',(-1.98819231399505,8.37030423910157,-0.333570656303743));
#3712=CARTESIAN_POINT('Ctrl Pts',(-1.83984508919913,8.34106611245623,-0.82668715605278));
#3713=CARTESIAN_POINT('Ctrl Pts',(-1.71605288881846,8.32566902073102,-1.05999906906072));
#3714=CARTESIAN_POINT('Ctrl Pts',(-1.38205991004181,8.29520673661087,-1.47016497640736));
#3715=CARTESIAN_POINT('Ctrl Pts',(-1.1734417375009,8.2809507699327,-1.64147268846638));
#3716=CARTESIAN_POINT('Ctrl Pts',(-0.712101744651061,8.2540392703498,-1.88625652499066));
#3717=CARTESIAN_POINT('Ctrl Pts',(-0.466038132703796,8.23968555965287,-1.96158530310034));
#3718=CARTESIAN_POINT('Ctrl Pts',(0.0509150518454933,8.20952995722083,-2.01682795565735));
#3719=CARTESIAN_POINT('Ctrl Pts',(0.317346157923531,8.19398814269962,-1.99235909767874));
#3720=CARTESIAN_POINT('Ctrl Pts',(0.818350872074179,8.16476286770749,-1.84303438253474));
#3721=CARTESIAN_POINT('Ctrl Pts',(1.04882097278607,8.15225195365897,-1.72233608337629));
#3722=CARTESIAN_POINT('Ctrl Pts',(1.45145272527099,8.12422186462602,-1.39994376724921));
#3723=CARTESIAN_POINT('Ctrl Pts',(1.6197241441659,8.10927675151018,-1.20125879919931));
#3724=CARTESIAN_POINT('Ctrl Pts',(1.87504113665927,8.07876436630004,-0.744677545611848));
#3725=CARTESIAN_POINT('Ctrl Pts',(1.95716921969409,8.06349017467688,-0.48974363433592));
#3726=CARTESIAN_POINT('Ctrl Pts',(2.01584665253484,8.03573648438144,0.0257595247521755));
#3727=CARTESIAN_POINT('Ctrl Pts',(1.99635790625494,8.02320603143971,0.280844471619683));
#3728=CARTESIAN_POINT('Ctrl Pts',(1.8611518568783,7.99418245413774,0.777301056952316));
#3729=CARTESIAN_POINT('Ctrl Pts',(1.74398071264898,7.97884704441316,1.0132146515514));
#3730=CARTESIAN_POINT('Ctrl Pts',(1.4230787837332,7.94842748141968,1.43009302106559));
#3731=CARTESIAN_POINT('Ctrl Pts',(1.22120597579789,7.9337370171667,1.6058827908322));
#3732=CARTESIAN_POINT('Ctrl Pts',(0.770197508503904,7.90742818990788,1.86318425309167));
#3733=CARTESIAN_POINT('Ctrl Pts',(0.527356863978595,7.89326248564391,1.94589485813412));
#3734=CARTESIAN_POINT('Ctrl Pts',(0.184077252924329,7.87323784166574,1.99365311316229));
#3735=CARTESIAN_POINT('Ctrl Pts',(0.0919931555425928,7.86786626931849,2.));
#3736=CARTESIAN_POINT('Ctrl Pts',(7.41933818794109E-16,7.86250000191184,
2.));
#3737=CARTESIAN_POINT('Origin',(0.,70.,0.));
#3738=CARTESIAN_POINT('',(1.15522243134092E-14,7.07500000000001,2.));
#3739=CARTESIAN_POINT('',(2.77424798298637E-14,7.16250000191184,2.));
#3740=CARTESIAN_POINT('',(-2.44929359829471E-16,70.,2.));
#3741=CARTESIAN_POINT('Ctrl Pts',(2.77555756156289E-15,7.07500000000001,
2.));
#3742=CARTESIAN_POINT('Ctrl Pts',(0.18075001537359,7.0855437508968,2.));
#3743=CARTESIAN_POINT('Ctrl Pts',(0.361045488426424,7.09606098682489,1.97549558457209));
#3744=CARTESIAN_POINT('Ctrl Pts',(0.780464168592415,7.12052707650124,1.85884827886082));
#3745=CARTESIAN_POINT('Ctrl Pts',(1.00980068654218,7.13296927010253,1.74491581958734));
#3746=CARTESIAN_POINT('Ctrl Pts',(1.424797160282,7.16103928503801,1.42887195069992));
#3747=CARTESIAN_POINT('Ctrl Pts',(1.60308448387472,7.1765141876913,1.22548255482433));
#3748=CARTESIAN_POINT('Ctrl Pts',(1.86388487381245,7.20715280130596,0.769568467827498));
#3749=CARTESIAN_POINT('Ctrl Pts',(1.94739624750753,7.22202289434249,0.523432277310207));
#3750=CARTESIAN_POINT('Ctrl Pts',(2.01664966892294,7.2498957261951,0.0116767768689988));
#3751=CARTESIAN_POINT('Ctrl Pts',(2.00124002591604,7.2625490039063,-0.249121784725706));
#3752=CARTESIAN_POINT('Ctrl Pts',(1.87045356876465,7.29196387648333,-0.755875660500865));
#3753=CARTESIAN_POINT('Ctrl Pts',(1.7542241045094,7.30750009794585,-0.996307975805123));
#3754=CARTESIAN_POINT('Ctrl Pts',(1.44098348851282,7.33753973800396,-1.41008908265801));
#3755=CARTESIAN_POINT('Ctrl Pts',(1.24999174383528,7.35178900326569,-1.58188224921385));
#3756=CARTESIAN_POINT('Ctrl Pts',(0.804853188205148,7.37831632268762,-1.84998612746433));
#3757=CARTESIAN_POINT('Ctrl Pts',(0.552818933868428,7.3927522288577,-1.94028996818693));
#3758=CARTESIAN_POINT('Ctrl Pts',(0.0319492719416979,7.42313629247009,-2.01673692536205));
#3759=CARTESIAN_POINT('Ctrl Pts',(-0.2314801387626,7.43850300809451,-2.00366511395298));
#3760=CARTESIAN_POINT('Ctrl Pts',(-0.73082548624653,7.46763148669773,-1.87886356825441));
#3761=CARTESIAN_POINT('Ctrl Pts',(-0.962733721555366,7.48026571814896,-1.77125814433366));
#3762=CARTESIAN_POINT('Ctrl Pts',(-1.38366999666347,7.5078495257626,-1.4682680303301));
#3763=CARTESIAN_POINT('Ctrl Pts',(-1.56595192662907,7.52307867990314,-1.27204948049025));
#3764=CARTESIAN_POINT('Ctrl Pts',(-1.83971471151476,7.55360098365991,-0.825921573800778));
#3765=CARTESIAN_POINT('Ctrl Pts',(-1.93089668745128,7.56859866822386,-0.581688350316966));
#3766=CARTESIAN_POINT('Ctrl Pts',(-2.01512890183861,7.59674314815885,-0.073203622539262));
#3767=CARTESIAN_POINT('Ctrl Pts',(-2.0078505381786,7.60917390033838,0.186128641640483));
#3768=CARTESIAN_POINT('Ctrl Pts',(-1.89369140290797,7.63825805879553,0.695935864369098));
#3769=CARTESIAN_POINT('Ctrl Pts',(-1.78477579336675,7.65380071724004,0.940718254859585));
#3770=CARTESIAN_POINT('Ctrl Pts',(-1.48359922254668,7.68403526170145,1.36532264806138));
#3771=CARTESIAN_POINT('Ctrl Pts',(-1.29736617565955,7.6984627489118,1.54339112972496));
#3772=CARTESIAN_POINT('Ctrl Pts',(-0.859053556344717,7.7255025169672,1.82557981636653));
#3773=CARTESIAN_POINT('Ctrl Pts',(-0.608949336314592,7.73947795538168,1.92352746147435));
#3774=CARTESIAN_POINT('Ctrl Pts',(-0.232127609363206,7.76145922278717,1.9899015910211));
#3775=CARTESIAN_POINT('Ctrl Pts',(-0.116037570983665,7.76823114169263,2.));
#3776=CARTESIAN_POINT('Ctrl Pts',(-1.30451205393456E-14,7.77500000000001,
2.));
#3777=CARTESIAN_POINT('Ctrl Pts',(-8.81239525796218E-15,7.86250000191184,
2.));
#3778=CARTESIAN_POINT('Ctrl Pts',(-0.170927915536333,7.85252920683889,2.));
#3779=CARTESIAN_POINT('Ctrl Pts',(-0.341541867911621,7.84257672628365,1.97808665376321));
#3780=CARTESIAN_POINT('Ctrl Pts',(-0.758885913122223,7.81823165697969,1.86857667624832));
#3781=CARTESIAN_POINT('Ctrl Pts',(-0.994861517242304,7.80544273906337,1.75434374789522));
#3782=CARTESIAN_POINT('Ctrl Pts',(-1.40796857062281,7.77769218627607,1.44353273218894));
#3783=CARTESIAN_POINT('Ctrl Pts',(-1.58173289424033,7.76288250550425,1.25069995931156));
#3784=CARTESIAN_POINT('Ctrl Pts',(-1.85193784129827,7.73229012686178,0.801130810995777));
#3785=CARTESIAN_POINT('Ctrl Pts',(-1.94234540788994,7.71679662924098,0.54663592886225));
#3786=CARTESIAN_POINT('Ctrl Pts',(-2.01585596229509,7.68856662216761,0.0302680495322416));
#3787=CARTESIAN_POINT('Ctrl Pts',(-2.00339738064947,7.67619058053996,-0.225829963435849));
#3788=CARTESIAN_POINT('Ctrl Pts',(-1.88179826829948,7.64739455891102,-0.725638083383513));
#3789=CARTESIAN_POINT('Ctrl Pts',(-1.77152704155437,7.63213418936647,-0.964049936863562));
#3790=CARTESIAN_POINT('Ctrl Pts',(-1.46304234590713,7.60166108043189,-1.3891573340967));
#3791=CARTESIAN_POINT('Ctrl Pts',(-1.26624422002002,7.58675269938869,-1.57064529371589));
#3792=CARTESIAN_POINT('Ctrl Pts',(-0.823160978616651,7.56020718367607,-1.84029600133115));
#3793=CARTESIAN_POINT('Ctrl Pts',(-0.583407349987985,7.5465320973278,-1.92976747259992));
#3794=CARTESIAN_POINT('Ctrl Pts',(-0.0736314799885643,7.51679517157783,
-2.01591269398287));
#3795=CARTESIAN_POINT('Ctrl Pts',(0.192116356904062,7.50129321442576,-2.00808913417545));
#3796=CARTESIAN_POINT('Ctrl Pts',(0.703897777311664,7.47143929823532,-1.89026446179254));
#3797=CARTESIAN_POINT('Ctrl Pts',(0.945012887021492,7.45829339178382,-1.7819919174932));
#3798=CARTESIAN_POINT('Ctrl Pts',(1.36754933020624,7.43080230809323,-1.48176111862576));
#3799=CARTESIAN_POINT('Ctrl Pts',(1.54610675000263,7.41612637933859,-1.2943432444248));
#3800=CARTESIAN_POINT('Ctrl Pts',(1.82811837678127,7.3856478205279,-0.853843734184673));
#3801=CARTESIAN_POINT('Ctrl Pts',(1.92553893926196,7.37012516637964,-0.602820657550663));
#3802=CARTESIAN_POINT('Ctrl Pts',(2.01423887029515,7.34156875761561,-0.0887612910552623));
#3803=CARTESIAN_POINT('Ctrl Pts',(2.00914246080169,7.3292552201465,0.168482755517828));
#3804=CARTESIAN_POINT('Ctrl Pts',(1.90163687533782,7.30070050621638,0.671651123354299));
#3805=CARTESIAN_POINT('Ctrl Pts',(1.79854795643332,7.28552962113398,0.912438351228735));
#3806=CARTESIAN_POINT('Ctrl Pts',(1.5030122408241,7.25501617620551,1.34582029118175));
#3807=CARTESIAN_POINT('Ctrl Pts',(1.31156334985062,7.23997567820554,1.53301187052302));
#3808=CARTESIAN_POINT('Ctrl Pts',(0.876747931810209,7.21303104797744,1.81533642668372));
#3809=CARTESIAN_POINT('Ctrl Pts',(0.640051660201568,7.19983634875693,1.91168002068908));
#3810=CARTESIAN_POINT('Ctrl Pts',(0.262351243869515,7.17780382447089,1.98709445304633));
#3811=CARTESIAN_POINT('Ctrl Pts',(0.131176897671107,7.17015198760932,2.));
#3812=CARTESIAN_POINT('Ctrl Pts',(1.94635974004598E-14,7.16250000191184,
2.));
#3813=CARTESIAN_POINT('Origin',(0.,70.,0.));
#3814=CARTESIAN_POINT('',(-1.84411445862298E-14,6.37500000000001,2.));
#3815=CARTESIAN_POINT('',(-2.40529750310148E-14,6.46250000191183,2.));
#3816=CARTESIAN_POINT('',(-2.44929359829471E-16,70.,2.));
#3817=CARTESIAN_POINT('Ctrl Pts',(-1.17961196366423E-15,6.37500000000001,
2.));
#3818=CARTESIAN_POINT('Ctrl Pts',(0.218380548180877,6.38773886531056,2.));
#3819=CARTESIAN_POINT('Ctrl Pts',(0.435591688754577,6.40040951517736,1.96422966283633));
#3820=CARTESIAN_POINT('Ctrl Pts',(0.884929306534349,6.42662087621452,1.81168954605897));
#3821=CARTESIAN_POINT('Ctrl Pts',(1.10891682053198,6.438941027859,1.68393039943082));
#3822=CARTESIAN_POINT('Ctrl Pts',(1.50482320290809,6.46765999926712,1.34401885449842));
#3823=CARTESIAN_POINT('Ctrl Pts',(1.67015368308462,6.48319254064221,1.13200787079262));
#3824=CARTESIAN_POINT('Ctrl Pts',(1.90358767799519,6.51360412968123,0.664787709398107));
#3825=CARTESIAN_POINT('Ctrl Pts',(1.9730051297779,6.52820790949486,0.415786023931368));
#3826=CARTESIAN_POINT('Ctrl Pts',(2.01464938398039,6.55556436137238,-0.101687964028044));
#3827=CARTESIAN_POINT('Ctrl Pts',(1.98385038468369,6.56893096680269,-0.365411973405472));
#3828=CARTESIAN_POINT('Ctrl Pts',(1.82194588911147,6.59893251064738,-0.865812920669644));
#3829=CARTESIAN_POINT('Ctrl Pts',(1.69248158566176,6.61441563030838,-1.0975529549371));
#3830=CARTESIAN_POINT('Ctrl Pts',(1.35744755693107,6.64403843999516,-1.49050052758113));
#3831=CARTESIAN_POINT('Ctrl Pts',(1.15786121375317,6.65745809586443,-1.6503169834607));
#3832=CARTESIAN_POINT('Ctrl Pts',(0.699330416206954,6.68420572572129,-1.89241907057509));
#3833=CARTESIAN_POINT('Ctrl Pts',(0.442588821013814,6.69918231877421,-1.96834453019336));
#3834=CARTESIAN_POINT('Ctrl Pts',(-0.0802124617398179,6.72967906026817,
-2.0152105369091));
#3835=CARTESIAN_POINT('Ctrl Pts',(-0.341071598113087,6.74489584322328,-1.98776130908745));
#3836=CARTESIAN_POINT('Ctrl Pts',(-0.832646432250627,6.7735710418813,-1.83616520518011));
#3837=CARTESIAN_POINT('Ctrl Pts',(-1.05930402513081,6.78590309899885,-1.71542183448551));
#3838=CARTESIAN_POINT('Ctrl Pts',(-1.46493654415258,6.81429808767927,-1.38753887196545));
#3839=CARTESIAN_POINT('Ctrl Pts',(-1.6368748729707,6.8298078339344,-1.17979415780545));
#3840=CARTESIAN_POINT('Ctrl Pts',(-1.88421942023241,6.86034603599379,-0.718098969736138));
#3841=CARTESIAN_POINT('Ctrl Pts',(-1.96078093250865,6.87508991725929,-0.470448619999976));
#3842=CARTESIAN_POINT('Ctrl Pts',(-2.01644214931359,6.9027110607266,0.0441722054775648));
#3843=CARTESIAN_POINT('Ctrl Pts',(-1.99352526301469,6.91566651786864,0.306378436585966));
#3844=CARTESIAN_POINT('Ctrl Pts',(-1.84749330568526,6.94537423800143,0.810127196963264));
#3845=CARTESIAN_POINT('Ctrl Pts',(-1.72470323726598,6.96089109295482,1.04638838822703));
#3846=CARTESIAN_POINT('Ctrl Pts',(-1.40063186189325,6.99073713004903,1.45008400843909));
#3847=CARTESIAN_POINT('Ctrl Pts',(-1.2054102831749,7.00468440014814,1.61598195763032));
#3848=CARTESIAN_POINT('Ctrl Pts',(-0.753718017516963,7.03103311564486,1.87141600842067));
#3849=CARTESIAN_POINT('Ctrl Pts',(-0.4993269770152,7.04587259300746,1.95471461206462));
#3850=CARTESIAN_POINT('Ctrl Pts',(-0.157628533769269,7.06580500219681,1.99534645887765));
#3851=CARTESIAN_POINT('Ctrl Pts',(-0.0787711029033106,7.07040501899732,
2.));
#3852=CARTESIAN_POINT('Ctrl Pts',(7.06522986662669E-16,7.07500000000001,
2.));
#3853=CARTESIAN_POINT('Ctrl Pts',(7.28583859910259E-16,7.16250000191184,
2.));
#3854=CARTESIAN_POINT('Ctrl Pts',(-0.130085342337019,7.15491169027551,2.));
#3855=CARTESIAN_POINT('Ctrl Pts',(-0.260173193860504,7.14732323226997,1.98730835440023));
#3856=CARTESIAN_POINT('Ctrl Pts',(-0.647613436418503,7.12472255145409,1.91060868087785));
#3857=CARTESIAN_POINT('Ctrl Pts',(-0.894039501496567,7.11111652008545,1.80844586712125));
#3858=CARTESIAN_POINT('Ctrl Pts',(-1.32599961792236,7.08389237484571,1.51893983950038));
#3859=CARTESIAN_POINT('Ctrl Pts',(-1.50919536615133,7.06936117580825,1.33706481088031));
#3860=CARTESIAN_POINT('Ctrl Pts',(-1.80274755706425,7.03902033480642,0.905954354073171));
#3861=CARTESIAN_POINT('Ctrl Pts',(-1.90707273670512,7.02348138496407,0.658595088928268));
#3862=CARTESIAN_POINT('Ctrl Pts',(-2.01097324670968,6.99460692224855,0.147015945325011));
#3863=CARTESIAN_POINT('Ctrl Pts',(-2.01325706028901,6.98225626544635,-0.111453029951849));
#3864=CARTESIAN_POINT('Ctrl Pts',(-1.91969827815215,6.95394570843383,-0.617840534886077));
#3865=CARTESIAN_POINT('Ctrl Pts',(-1.82374050019459,6.93887488292517,-0.860764263014212));
#3866=CARTESIAN_POINT('Ctrl Pts',(-1.54119962505294,6.90834755189457,-1.30192365114519));
#3867=CARTESIAN_POINT('Ctrl Pts',(-1.35519670898698,6.89318956543488,-1.49458513392608));
#3868=CARTESIAN_POINT('Ctrl Pts',(-0.928663878567721,6.86585886200204,-1.78933391177686));
#3869=CARTESIAN_POINT('Ctrl Pts',(-0.694874058553572,6.85303432199413,-1.89243627183466));
#3870=CARTESIAN_POINT('Ctrl Pts',(-0.192898216433379,6.82375239787045,-2.00781138139783));
#3871=CARTESIAN_POINT('Ctrl Pts',(0.0712480461586881,6.80834386588591,-2.0157963318781));
#3872=CARTESIAN_POINT('Ctrl Pts',(0.592606320201799,6.77793129990006,-1.92873446867424));
#3873=CARTESIAN_POINT('Ctrl Pts',(0.844272547940869,6.76378702629052,-1.83257521656462));
#3874=CARTESIAN_POINT('Ctrl Pts',(1.28524275043711,6.73682548011264,-1.55346927790099));
#3875=CARTESIAN_POINT('Ctrl Pts',(1.47272450383278,6.72244283300577,-1.37700934113293));
#3876=CARTESIAN_POINT('Ctrl Pts',(1.77705222671155,6.69225595917844,-0.95516790025197));
#3877=CARTESIAN_POINT('Ctrl Pts',(1.88787211036145,6.67671349033682,-0.71148869609447));
#3878=CARTESIAN_POINT('Ctrl Pts',(2.0063256635788,6.64754281569382,-0.202448280385498));
#3879=CARTESIAN_POINT('Ctrl Pts',(2.01569937528843,6.63506547903315,0.0572550936125673));
#3880=CARTESIAN_POINT('Ctrl Pts',(1.93535184143689,6.6069908702112,0.566599553397501));
#3881=CARTESIAN_POINT('Ctrl Pts',(1.8461595770448,6.59202509099077,0.811349975365595));
#3882=CARTESIAN_POINT('Ctrl Pts',(1.57607152285567,6.5615082351801,1.25949164744684));
#3883=CARTESIAN_POINT('Ctrl Pts',(1.39535709278812,6.54625119348052,1.45716722427951));
#3884=CARTESIAN_POINT('Ctrl Pts',(0.976765707076176,6.51856319528433,1.76357359946584));
#3885=CARTESIAN_POINT('Ctrl Pts',(0.745627243960202,6.50599492447618,1.87305159405641));
#3886=CARTESIAN_POINT('Ctrl Pts',(0.336420990336705,6.48212455968148,1.97874051917636));
#3887=CARTESIAN_POINT('Ctrl Pts',(0.168358723701333,6.47232092746108,2.));
#3888=CARTESIAN_POINT('Ctrl Pts',(-1.93942084614207E-14,6.46250000191184,
2.));
#3889=CARTESIAN_POINT('Origin',(0.,70.,0.));
#3890=CARTESIAN_POINT('',(-4.66744018697397E-15,5.67500000000001,2.));
#3891=CARTESIAN_POINT('',(-1.75217411439621E-14,5.76250000191184,2.));
#3892=CARTESIAN_POINT('',(-2.44929359829471E-16,70.,2.));
#3893=CARTESIAN_POINT('Ctrl Pts',(-2.82412981889024E-14,5.67500000000001,
2.));
#3894=CARTESIAN_POINT('Ctrl Pts',(0.256622987290695,5.68996967425863,2.));
#3895=CARTESIAN_POINT('Ctrl Pts',(0.510903094812502,5.70480268053074,1.95060829662963));
#3896=CARTESIAN_POINT('Ctrl Pts',(0.98864487151693,5.73267095083849,1.75767422282175));
#3897=CARTESIAN_POINT('Ctrl Pts',(1.20729575864517,5.74527608905864,1.61532781592622));
#3898=CARTESIAN_POINT('Ctrl Pts',(1.58274048039481,5.77463261224839,1.25098247340035));
#3899=CARTESIAN_POINT('Ctrl Pts',(1.73418273505864,5.79017111479687,1.03083511832571));
#3900=CARTESIAN_POINT('Ctrl Pts',(1.93867276023932,5.82024768614334,0.5535357786726));
#3901=CARTESIAN_POINT('Ctrl Pts',(1.99335332242581,5.8345297636046,0.302393801107101));
#3902=CARTESIAN_POINT('Ctrl Pts',(2.00575387368111,5.86114343640657,-0.217260834076487));
#3903=CARTESIAN_POINT('Ctrl Pts',(1.95934408693273,5.87548241404785,-0.480948278564949));
#3904=CARTESIAN_POINT('Ctrl Pts',(1.76766966346345,5.90585080865594,-0.971423311783889));
#3905=CARTESIAN_POINT('Ctrl Pts',(1.62571995226474,5.92122936175023,-1.19388501131151));
#3906=CARTESIAN_POINT('Ctrl Pts',(1.26980990061511,5.950399530426,-1.56581983817613));
#3907=CARTESIAN_POINT('Ctrl Pts',(1.06147049699314,5.96308088767541,-1.71390324343442));
#3908=CARTESIAN_POINT('Ctrl Pts',(0.589774685924296,5.99059647665443,-1.929382466369));
#3909=CARTESIAN_POINT('Ctrl Pts',(0.329024203695872,6.00580692145109,-1.99049109052132));
#3910=CARTESIAN_POINT('Ctrl Pts',(-0.194257962683431,6.03633171448988,-2.00724376634386));
#3911=CARTESIAN_POINT('Ctrl Pts',(-0.451709422575361,6.05134971631691,-1.96538755078824));
#3912=CARTESIAN_POINT('Ctrl Pts',(-0.934962207318963,6.07953946209362,-1.78656451965216));
#3913=CARTESIAN_POINT('Ctrl Pts',(-1.15638485129736,6.09194407065691,-1.65189124887631));
#3914=CARTESIAN_POINT('Ctrl Pts',(-1.54263006545917,6.12097164144872,-1.30029314231204));
#3915=CARTESIAN_POINT('Ctrl Pts',(-1.70139491179651,6.13651387264503,-1.08429967942574));
#3916=CARTESIAN_POINT('Ctrl Pts',(-1.92109767821886,6.16677837403545,-0.612063369916115));
#3917=CARTESIAN_POINT('Ctrl Pts',(-1.98350264718633,6.18123453238429,-0.361935172777406));
#3918=CARTESIAN_POINT('Ctrl Pts',(-2.01132046858475,6.20832476822178,0.158251798944814));
#3919=CARTESIAN_POINT('Ctrl Pts',(-1.97259634046109,6.22219505710803,0.423526679365465));
#3920=CARTESIAN_POINT('Ctrl Pts',(-1.7948926351988,6.25247731484111,0.920362642571417));
#3921=CARTESIAN_POINT('Ctrl Pts',(-1.65895060736644,6.26791324593325,1.14742866950801));
#3922=CARTESIAN_POINT('Ctrl Pts',(-1.31315585809985,6.29730720024909,1.52963337576748));
#3923=CARTESIAN_POINT('Ctrl Pts',(-1.1091346462743,6.31030047896735,1.68342957030648));
#3924=CARTESIAN_POINT('Ctrl Pts',(-0.643837424469834,6.33744281690594,1.91201655428822));
#3925=CARTESIAN_POINT('Ctrl Pts',(-0.38494640051787,6.35254479330314,1.98043092804347));
#3926=CARTESIAN_POINT('Ctrl Pts',(-0.0801986050553553,6.37032174803845,
1.99879523621637));
#3927=CARTESIAN_POINT('Ctrl Pts',(-0.0400796075752101,6.37266202289145,
2.));
#3928=CARTESIAN_POINT('Ctrl Pts',(7.06522986662669E-16,6.37500000000001,
2.));
#3929=CARTESIAN_POINT('Ctrl Pts',(7.41933818794109E-16,6.46250000191184,
2.));
#3930=CARTESIAN_POINT('Ctrl Pts',(-0.0915607604235562,6.4571589575538,2.));
#3931=CARTESIAN_POINT('Ctrl Pts',(-0.183209202623249,6.45181279842548,1.9937126289666));
#3932=CARTESIAN_POINT('Ctrl Pts',(-0.536976989776565,6.43117634417487,1.94473142989058));
#3933=CARTESIAN_POINT('Ctrl Pts',(-0.789715492509543,6.41658655291459,1.856492941354));
#3934=CARTESIAN_POINT('Ctrl Pts',(-1.23682283738656,6.39019265575449,1.59216681994931));
#3935=CARTESIAN_POINT('Ctrl Pts',(-1.42908114885385,6.37599432609523,1.4221131695151));
#3936=CARTESIAN_POINT('Ctrl Pts',(-1.74555908957954,6.34601287342013,1.01135294443712));
#3937=CARTESIAN_POINT('Ctrl Pts',(-1.86376231924679,6.33048108973694,0.772148028373824));
#3938=CARTESIAN_POINT('Ctrl Pts',(-1.99910065587187,6.300977719091,0.266270373989555));
#3939=CARTESIAN_POINT('Ctrl Pts',(-2.01674596082411,6.28824391348039,0.00505734510263627));
#3940=CARTESIAN_POINT('Ctrl Pts',(-1.95156457334202,6.26044596836682,-0.5075667722337));
#3941=CARTESIAN_POINT('Ctrl Pts',(-1.8701369046458,6.24561266472461,-0.754177749248546));
#3942=CARTESIAN_POINT('Ctrl Pts',(-1.61336286469494,6.21500178306147,-1.21186750021966));
#3943=CARTESIAN_POINT('Ctrl Pts',(-1.43697083813152,6.19951511201499,-1.41658410011584));
#3944=CARTESIAN_POINT('Ctrl Pts',(-1.02477287316995,6.17134663556016,-1.73619272141809));
#3945=CARTESIAN_POINT('Ctrl Pts',(-0.796248904014463,6.15894785464601,-1.85216696661008));
#3946=CARTESIAN_POINT('Ctrl Pts',(-0.301840294904721,6.13010735244795,-1.99416116119649));
#3947=CARTESIAN_POINT('Ctrl Pts',(-0.0399698268648906,6.11483157514562,
-2.01647577831176));
#3948=CARTESIAN_POINT('Ctrl Pts',(0.482246501087751,6.08436895601506,-1.95900073504723));
#3949=CARTESIAN_POINT('Ctrl Pts',(0.737369936774645,6.06948675559999,-1.87791959018816));
#3950=CARTESIAN_POINT('Ctrl Pts',(1.19114008483323,6.04301683029658,-1.62650353527467));
#3951=CARTESIAN_POINT('Ctrl Pts',(1.38767659175461,6.02923991067642,-1.46245415041243));
#3952=CARTESIAN_POINT('Ctrl Pts',(1.71508941030679,5.99946084104511,-1.06201332529899));
#3953=CARTESIAN_POINT('Ctrl Pts',(1.83992077022183,5.98395276040648,-0.827104360618089));
#3954=CARTESIAN_POINT('Ctrl Pts',(1.99076641106456,5.95415471494468,-0.324346803895114));
#3955=CARTESIAN_POINT('Ctrl Pts',(2.01606600444625,5.94108482252657,-0.0616853330448833));
#3956=CARTESIAN_POINT('Ctrl Pts',(1.96466974215094,5.91354366508803,0.453814552315483));
#3957=CARTESIAN_POINT('Ctrl Pts',(1.89028497862779,5.89884136498054,0.701898555063765));
#3958=CARTESIAN_POINT('Ctrl Pts',(1.6471704709921,5.86833924208025,1.16532177551644));
#3959=CARTESIAN_POINT('Ctrl Pts',(1.47723680651845,5.85282115977933,1.3743888940881));
#3960=CARTESIAN_POINT('Ctrl Pts',(1.0745560612086,5.82432638399933,1.70595133625727));
#3961=CARTESIAN_POINT('Ctrl Pts',(0.848720261100305,5.81200868380936,1.82882984987381));
#3962=CARTESIAN_POINT('Ctrl Pts',(0.409621056617632,5.78639456354787,1.96840229651907));
#3963=CARTESIAN_POINT('Ctrl Pts',(0.205248527642598,5.77447283269099,2.));
#3964=CARTESIAN_POINT('Ctrl Pts',(2.28983498828939E-15,5.76250000191184,
2.));
#3965=CARTESIAN_POINT('Origin',(0.,70.,0.));
#3966=CARTESIAN_POINT('',(3.10331689486287E-14,4.97500000000001,2.));
#3967=CARTESIAN_POINT('',(-3.30631497031952E-16,5.06250000191184,2.));
#3968=CARTESIAN_POINT('',(-2.44929359829471E-16,70.,2.));
#3969=CARTESIAN_POINT('Ctrl Pts',(7.06522986662669E-16,4.97500000000001,
2.));
#3970=CARTESIAN_POINT('Ctrl Pts',(0.0362596285020658,4.97711514499596,2.));
#3971=CARTESIAN_POINT('Ctrl Pts',(0.0725542216904652,4.97923232959862,1.99901394277815));
#3972=CARTESIAN_POINT('Ctrl Pts',(0.364710195054145,4.99627476137817,1.98309063559847));
#3973=CARTESIAN_POINT('Ctrl Pts',(0.61556521188284,5.01090797069318,1.92009875767504));
#3974=CARTESIAN_POINT('Ctrl Pts',(1.08546753210051,5.03831893937254,1.7001948362507));
#3975=CARTESIAN_POINT('Ctrl Pts',(1.29899833487608,5.05159334250551,1.54322313517846));
#3976=CARTESIAN_POINT('Ctrl Pts',(1.65364486511862,5.08153556301639,1.15527615098086));
#3977=CARTESIAN_POINT('Ctrl Pts',(1.7910990033383,5.09702672449809,0.92798986320257));
#3978=CARTESIAN_POINT('Ctrl Pts',(1.96691498867721,5.12669588188906,0.442200263735244));
#3979=CARTESIAN_POINT('Ctrl Pts',(2.00705569561547,5.14021574498876,0.189604412736546));
#3980=CARTESIAN_POINT('Ctrl Pts',(1.99054196800901,5.16688173088232,-0.328711009630941));
#3981=CARTESIAN_POINT('Ctrl Pts',(1.92948015500898,5.18183108715165,-0.589377465160195));
#3982=CARTESIAN_POINT('Ctrl Pts',(1.71145619097226,5.21231906344031,-1.06700668742727));
#3983=CARTESIAN_POINT('Ctrl Pts',(1.55841129512922,5.22755387528183,-1.28021724022294));
#3984=CARTESIAN_POINT('Ctrl Pts',(1.18337201187085,5.25627821511708,-1.63228267774596));
#3985=CARTESIAN_POINT('Ctrl Pts',(0.96642767135054,5.26862505250456,-1.76938598269431));
#3986=CARTESIAN_POINT('Ctrl Pts',(0.480800266469448,5.29695331778929,-1.95964812161272));
#3987=CARTESIAN_POINT('Ctrl Pts',(0.215025294473574,5.31245685782238,-2.00627095256879));
#3988=CARTESIAN_POINT('Ctrl Pts',(-0.308876250480484,5.34301778127804,-1.99264086171038));
#3989=CARTESIAN_POINT('Ctrl Pts',(-0.562092181003058,5.35778871055852,-1.93651970495745));
#3990=CARTESIAN_POINT('Ctrl Pts',(-1.03650185539069,5.38546260823113,-1.73015564751182));
#3991=CARTESIAN_POINT('Ctrl Pts',(-1.25264836203467,5.39834736740584,-1.58071660922677));
#3992=CARTESIAN_POINT('Ctrl Pts',(-1.61804096069133,5.42799478922013,-1.20480937132668));
#3993=CARTESIAN_POINT('Ctrl Pts',(-1.76269945501799,5.44351674674541,-0.981072916918595));
#3994=CARTESIAN_POINT('Ctrl Pts',(-1.95324518871418,5.47340670783459,-0.499416761929923));
#3995=CARTESIAN_POINT('Ctrl Pts',(-2.000799555136,5.48747150510802,-0.247538258858837));
#3996=CARTESIAN_POINT('Ctrl Pts',(-1.9991444128466,5.51373996717858,0.271486840785107));
#3997=CARTESIAN_POINT('Ctrl Pts',(-1.94559635272304,5.52855066299585,0.53374659844057));
#3998=CARTESIAN_POINT('Ctrl Pts',(-1.74112500106917,5.55898103606433,1.01806017706896));
#3999=CARTESIAN_POINT('Ctrl Pts',(-1.59373661025392,5.5742955484624,1.23611417643179));
#4000=CARTESIAN_POINT('Ctrl Pts',(-1.22853150879851,5.60325276527767,1.59846715016656));
#4001=CARTESIAN_POINT('Ctrl Pts',(-1.01608589317159,5.61572832289833,1.74124724903627));
#4002=CARTESIAN_POINT('Ctrl Pts',(-0.53600079059646,5.64373328721522,1.94538128070972));
#4003=CARTESIAN_POINT('Ctrl Pts',(-0.270859636694515,5.65919985452616,1.99960110895732));
#4004=CARTESIAN_POINT('Ctrl Pts',(-0.00197433811420763,5.67488483027668,
1.99999926914862));
#4005=CARTESIAN_POINT('Ctrl Pts',(-0.000987151723183884,5.67494241614949,
2.));
#4006=CARTESIAN_POINT('Ctrl Pts',(7.0652298666267E-16,5.67500000000001,
2.));
#4007=CARTESIAN_POINT('Ctrl Pts',(7.41933818794109E-16,5.76250000191184,
2.));
#4008=CARTESIAN_POINT('Ctrl Pts',(-0.0535565212988742,5.75937587150274,
2.));
#4009=CARTESIAN_POINT('Ctrl Pts',(-0.107172686776816,5.75624826184986,1.99784881882323));
#4010=CARTESIAN_POINT('Ctrl Pts',(-0.424952970807837,5.73771107861472,1.97222923346625));
#4011=CARTESIAN_POINT('Ctrl Pts',(-0.682377513849286,5.7226946469373,1.89859966741249));
#4012=CARTESIAN_POINT('Ctrl Pts',(-1.14299744186195,5.69582515113657,1.66063450329597));
#4013=CARTESIAN_POINT('Ctrl Pts',(-1.34393980807102,5.68254748379355,1.50267567444916));
#4014=CARTESIAN_POINT('Ctrl Pts',(-1.68230444135283,5.65299448637494,1.11303295175884));
#4015=CARTESIAN_POINT('Ctrl Pts',(-1.81378229442771,5.63752446314882,0.882714683088012));
#4016=CARTESIAN_POINT('Ctrl Pts',(-1.98055406188004,5.6074351644053,0.383386760058109));
#4017=CARTESIAN_POINT('Ctrl Pts',(-2.01378555634754,5.59392326899395,0.119188618895204));
#4018=CARTESIAN_POINT('Ctrl Pts',(-1.97641370238146,5.56664853380106,-0.399134469638205));
#4019=CARTESIAN_POINT('Ctrl Pts',(-1.90916731049059,5.55208939285681,-0.648505996663667));
#4020=CARTESIAN_POINT('Ctrl Pts',(-1.67997638436286,5.52172093793137,-1.11732206094771));
#4021=CARTESIAN_POINT('Ctrl Pts',(-1.51667023686694,5.50618405975824,-1.33058764000911));
#4022=CARTESIAN_POINT('Ctrl Pts',(-1.12374216379702,5.47736857298723,-1.67412922133258));
#4023=CARTESIAN_POINT('Ctrl Pts',(-0.900553375234095,5.46503228213383,-1.80402555433781));
#4024=CARTESIAN_POINT('Ctrl Pts',(-0.414442565133177,5.43667581821127,-1.97364496289496));
#4025=CARTESIAN_POINT('Ctrl Pts',(-0.155750888780536,5.42158547042404,-2.01066050345587));
#4026=CARTESIAN_POINT('Ctrl Pts',(0.367563861501855,5.39105877665756,-1.98373238228265));
#4027=CARTESIAN_POINT('Ctrl Pts',(0.627056522500649,5.37592170476597,-1.91758693942038));
#4028=CARTESIAN_POINT('Ctrl Pts',(1.09435980158698,5.34866234681927,-1.69307362107187));
#4029=CARTESIAN_POINT('Ctrl Pts',(1.29972095426504,5.33577658468415,-1.54106552793296));
#4030=CARTESIAN_POINT('Ctrl Pts',(1.64869242831578,5.30645201211671,-1.16206830702074));
#4031=CARTESIAN_POINT('Ctrl Pts',(1.78653036949275,5.29103273007053,-0.936426451804174));
#4032=CARTESIAN_POINT('Ctrl Pts',(1.96893851738666,5.26066923556934,-0.440698528848537));
#4033=CARTESIAN_POINT('Ctrl Pts',(2.0100395236924,5.24663127996597,-0.174956107182668));
#4034=CARTESIAN_POINT('Ctrl Pts',(1.98631606581007,5.21962086016237,0.346014798692541));
#4035=CARTESIAN_POINT('Ctrl Pts',(1.92597945494549,5.20521014024438,0.596437715271993));
#4036=CARTESIAN_POINT('Ctrl Pts',(1.71034122468579,5.17499330673269,1.07007710653928));
#4037=CARTESIAN_POINT('Ctrl Pts',(1.55352787914582,5.15945059907308,1.28720670046375));
#4038=CARTESIAN_POINT('Ctrl Pts',(1.17015730592201,5.13033381134792,1.64223051902134));
#4039=CARTESIAN_POINT('Ctrl Pts',(0.949481719457653,5.11788643554687,1.77895158304812));
#4040=CARTESIAN_POINT('Ctrl Pts',(0.482289331210749,5.09063354623247,1.95605222622256));
#4041=CARTESIAN_POINT('Ctrl Pts',(0.242062470307809,5.0766203126798,2.));
#4042=CARTESIAN_POINT('Ctrl Pts',(1.8249290967276E-14,5.06250000191184,
2.));
#4043=CARTESIAN_POINT('Origin',(0.,70.,0.));
#4044=CARTESIAN_POINT('',(3.07729604272322E-14,4.27500000000001,2.));
#4045=CARTESIAN_POINT('',(-9.5940548587481E-15,4.36250000191184,2.));
#4046=CARTESIAN_POINT('',(-2.44929359829471E-16,70.,2.));
#4047=CARTESIAN_POINT('Ctrl Pts',(7.0652298666267E-16,4.27500000000001,
2.));
#4048=CARTESIAN_POINT('Ctrl Pts',(0.0660280436593563,4.27885163588014,2.));
#4049=CARTESIAN_POINT('Ctrl Pts',(0.132131846816979,4.28270769106434,1.99673030440369));
#4050=CARTESIAN_POINT('Ctrl Pts',(0.461823825134132,4.30193972313284,1.96391816789203));
#4051=CARTESIAN_POINT('Ctrl Pts',(0.717794879749972,4.31687136798543,1.88549083015052));
#4052=CARTESIAN_POINT('Ctrl Pts',(1.17402763380875,4.34348494530552,1.6388735121033));
#4053=CARTESIAN_POINT('Ctrl Pts',(1.37213504547016,4.35707126239266,1.47701394256362));
#4054=CARTESIAN_POINT('Ctrl Pts',(1.70349591608626,4.38676999221564,1.08044284214248));
#4055=CARTESIAN_POINT('Ctrl Pts',(1.8307315019229,4.40226600685819,0.847160802724497));
#4056=CARTESIAN_POINT('Ctrl Pts',(1.98729226136375,4.43216992419419,0.345607151660183));
#4057=CARTESIAN_POINT('Ctrl Pts',(2.01542930392403,4.44538731856774,0.0823992975103338));
#4058=CARTESIAN_POINT('Ctrl Pts',(1.96829235486285,4.47330001037226,-0.442914176380998));
#4059=CARTESIAN_POINT('Ctrl Pts',(1.8922780240453,4.48848985463503,-0.699708217371228));
#4060=CARTESIAN_POINT('Ctrl Pts',(1.64767567224347,4.51901639054792,-1.16275568291626));
#4061=CARTESIAN_POINT('Ctrl Pts',(1.48372605197918,4.53405583238078,-1.3658030669174));
#4062=CARTESIAN_POINT('Ctrl Pts',(1.08912209056416,4.56229404554539,-1.69695001975465));
#4063=CARTESIAN_POINT('Ctrl Pts',(0.862727582973985,4.57467422432653,-1.82250652223345));
#4064=CARTESIAN_POINT('Ctrl Pts',(0.366158831456928,4.60364073483169,-1.98405622766587));
#4065=CARTESIAN_POINT('Ctrl Pts',(0.0997367074387389,4.61918202539941,-2.01508899181099));
#4066=CARTESIAN_POINT('Ctrl Pts',(-0.419619216201984,4.64947778761179,-1.97211248715117));
#4067=CARTESIAN_POINT('Ctrl Pts',(-0.667959623064703,4.66396431134545,-1.9024140392818));
#4068=CARTESIAN_POINT('Ctrl Pts',(-1.13328695123016,4.69110840548844,-1.66908381206157));
#4069=CARTESIAN_POINT('Ctrl Pts',(-1.34418864430199,4.70486981007299,-1.50445653481907));
#4070=CARTESIAN_POINT('Ctrl Pts',(-1.68783946026691,4.73509648447215,-1.10453044531571));
#4071=CARTESIAN_POINT('Ctrl Pts',(-1.81798635539873,4.75054300699671,-0.873908940965106));
#4072=CARTESIAN_POINT('Ctrl Pts',(-1.97904354795584,4.77998358540772,-0.384123038876249));
#4073=CARTESIAN_POINT('Ctrl Pts',(-2.01172361530772,4.79305470316162,-0.130712590377672));
#4074=CARTESIAN_POINT('Ctrl Pts',(-1.98009257935505,4.82011772909884,0.38673420455541));
#4075=CARTESIAN_POINT('Ctrl Pts',(-1.91142647080755,4.83519536864651,0.64554966835597));
#4076=CARTESIAN_POINT('Ctrl Pts',(-1.67982007339063,4.86571576749315,1.11597886925722));
#4077=CARTESIAN_POINT('Ctrl Pts',(-1.52117051331359,4.88085741078071,1.32410930857298));
#4078=CARTESIAN_POINT('Ctrl Pts',(-1.13618802742279,4.90933838299361,1.66561660581584));
#4079=CARTESIAN_POINT('Ctrl Pts',(-0.914523747015572,4.9216527814241,1.79689914786514));
#4080=CARTESIAN_POINT('Ctrl Pts',(-0.457540602005686,4.94831013154968,1.96050414645654));
#4081=CARTESIAN_POINT('Ctrl Pts',(-0.2294704759585,4.96161422223576,2.));
#4082=CARTESIAN_POINT('Ctrl Pts',(-1.26981758441502E-14,4.97500000000001,
2.));
#4083=CARTESIAN_POINT('Ctrl Pts',(7.41933818794109E-16,5.06250000191184,
2.));
#4084=CARTESIAN_POINT('Ctrl Pts',(-0.0158442249904296,5.06157575545407,
2.));
#4085=CARTESIAN_POINT('Ctrl Pts',(-0.0316963144127123,5.06065105023777,
1.99981172099515));
#4086=CARTESIAN_POINT('Ctrl Pts',(-0.312652205616501,5.04426195658421,1.9931296883174));
#4087=CARTESIAN_POINT('Ctrl Pts',(-0.573905474679356,5.02902218255555,1.93416331683831));
#4088=CARTESIAN_POINT('Ctrl Pts',(-1.04744463333177,5.00139906496749,1.72252415915947));
#4089=CARTESIAN_POINT('Ctrl Pts',(-1.25705308625539,4.98879057716396,1.57609280123643));
#4090=CARTESIAN_POINT('Ctrl Pts',(-1.61586906011901,4.95968623431236,1.20713872273769));
#4091=CARTESIAN_POINT('Ctrl Pts',(-1.75952803750774,4.94432653048774,0.986036987279413));
#4092=CARTESIAN_POINT('Ctrl Pts',(-1.95522856438524,4.9139338069324,0.497404837687051));
#4093=CARTESIAN_POINT('Ctrl Pts',(-2.00384801559129,4.89944067328008,0.234142341287129));
#4094=CARTESIAN_POINT('Ctrl Pts',(-1.99567467843145,4.87242379832758,-0.295934209782576));
#4095=CARTESIAN_POINT('Ctrl Pts',(-1.93891490850734,4.8575523994666,-0.55754129455507));
#4096=CARTESIAN_POINT('Ctrl Pts',(-1.72863461118595,4.82709432180272,-1.0390494856024));
#4097=CARTESIAN_POINT('Ctrl Pts',(-1.57881402037006,4.81181238639888,-1.25505439639258));
#4098=CARTESIAN_POINT('Ctrl Pts',(-1.20940297661085,4.78295381636324,-1.61302636838513));
#4099=CARTESIAN_POINT('Ctrl Pts',(-0.995053317087455,4.77054477874194,-1.75338750766115));
#4100=CARTESIAN_POINT('Ctrl Pts',(-0.512595717979786,4.74240141879399,-1.95163357121211));
#4101=CARTESIAN_POINT('Ctrl Pts',(-0.247159709890235,4.72691765165544,-2.00262490886725));
#4102=CARTESIAN_POINT('Ctrl Pts',(0.277723269735549,4.69629947784393,-1.99727141138786));
#4103=CARTESIAN_POINT('Ctrl Pts',(0.532171369632447,4.68145667201661,-1.94500612820907));
#4104=CARTESIAN_POINT('Ctrl Pts',(1.00903693678815,4.65363951393253,-1.74615634794997));
#4105=CARTESIAN_POINT('Ctrl Pts',(1.22662568191518,4.64092713874215,-1.60081848208624));
#4106=CARTESIAN_POINT('Ctrl Pts',(1.59783861761927,4.61144636305487,-1.23157035516275));
#4107=CARTESIAN_POINT('Ctrl Pts',(1.74642054344869,4.59591333276462,-1.00987991108583));
#4108=CARTESIAN_POINT('Ctrl Pts',(1.94499629944206,4.56591677140326,-0.53074975348895));
#4109=CARTESIAN_POINT('Ctrl Pts',(1.99668628473844,4.55170530119424,-0.279278826673935));
#4110=CARTESIAN_POINT('Ctrl Pts',(2.00313609598665,4.52527705508717,0.240140973207252));
#4111=CARTESIAN_POINT('Ctrl Pts',(1.95373188159054,4.51072735281215,0.50324810074014));
#4112=CARTESIAN_POINT('Ctrl Pts',(1.756603634623,4.48032647258704,0.991217415942218));
#4113=CARTESIAN_POINT('Ctrl Pts',(1.61233983702273,4.46497371538134,1.21183245089532));
#4114=CARTESIAN_POINT('Ctrl Pts',(1.25249235733571,4.43589290269783,1.5797252126963));
#4115=CARTESIAN_POINT('Ctrl Pts',(1.04243026343621,4.42330843394563,1.72556888955745));
#4116=CARTESIAN_POINT('Ctrl Pts',(0.568236339304095,4.39564712170459,1.9358368161416));
#4117=CARTESIAN_POINT('Ctrl Pts',(0.306808131447931,4.38039714291298,1.99403813371026));
#4118=CARTESIAN_POINT('Ctrl Pts',(0.0277872371021949,4.36412092407614,1.99985528997697));
#4119=CARTESIAN_POINT('Ctrl Pts',(0.0138905427157841,4.36331028357026,2.));
#4120=CARTESIAN_POINT('Ctrl Pts',(7.41933818794109E-16,4.36250000191184,
2.));
#4121=CARTESIAN_POINT('Origin',(0.,70.,0.));
#4122=CARTESIAN_POINT('',(2.19171970823706E-14,3.57500000000001,2.));
#4123=CARTESIAN_POINT('',(-1.89095199247436E-14,3.66250000191184,2.));
#4124=CARTESIAN_POINT('',(-2.44929359829471E-16,70.,2.));
#4125=CARTESIAN_POINT('Ctrl Pts',(-4.64905891561784E-15,3.57500000000001,
2.));
#4126=CARTESIAN_POINT('Ctrl Pts',(0.10288782586422,3.58100178984209,2.));
#4127=CARTESIAN_POINT('Ctrl Pts',(0.205854153830501,3.58700815897345,1.99206073891009));
#4128=CARTESIAN_POINT('Ctrl Pts',(0.57260818517212,3.60840214413505,1.93490351158503));
#4129=CARTESIAN_POINT('Ctrl Pts',(0.826191600282839,3.62276308212701,1.84093919135471));
#4130=CARTESIAN_POINT('Ctrl Pts',(1.27039250159657,3.64962865702265,1.56559823623058));
#4131=CARTESIAN_POINT('Ctrl Pts',(1.4593745191971,3.66395565023105,1.3911061388883));
#4132=CARTESIAN_POINT('Ctrl Pts',(1.76750162445167,3.69408203946287,0.972655556930503));
#4133=CARTESIAN_POINT('Ctrl Pts',(1.88062319441531,3.70962289434875,0.730337180024206));
#4134=CARTESIAN_POINT('Ctrl Pts',(2.00429943040821,3.73889776006813,0.222249633187286));
#4135=CARTESIAN_POINT('Ctrl Pts',(2.01622565796333,3.75144201407525,-0.0379123639191237));
#4136=CARTESIAN_POINT('Ctrl Pts',(1.94058731459248,3.77943137644466,-0.548288233958856));
#4137=CARTESIAN_POINT('Ctrl Pts',(1.85380691481358,3.79435735942738,-0.793643385403029));
#4138=CARTESIAN_POINT('Ctrl Pts',(1.58818698640604,3.82486498480195,-1.24418201585821));
#4139=CARTESIAN_POINT('Ctrl Pts',(1.40938613254919,3.84015444861909,-1.44360418791558));
#4140=CARTESIAN_POINT('Ctrl Pts',(0.993648361474997,3.86796776492616,-1.75413875354027));
#4141=CARTESIAN_POINT('Ctrl Pts',(0.763432480597549,3.88046643863182,-1.86588484710983));
#4142=CARTESIAN_POINT('Ctrl Pts',(0.266522971048555,3.90945282668884,-1.99924678864832));
#4143=CARTESIAN_POINT('Ctrl Pts',(0.00382923850926156,3.92477662775364,
-2.01692743821058));
#4144=CARTESIAN_POINT('Ctrl Pts',(-0.517842312609391,3.95520746823556,-1.94991132167082));
#4145=CARTESIAN_POINT('Ctrl Pts',(-0.771408032450691,3.96999176339004,-1.86416776779294));
#4146=CARTESIAN_POINT('Ctrl Pts',(-1.22084519606734,3.9962227458683,-1.60441164222163));
#4147=CARTESIAN_POINT('Ctrl Pts',(-1.41460864884182,4.01035849540025,-1.43646575078409));
#4148=CARTESIAN_POINT('Ctrl Pts',(-1.73494915944347,4.04026710313756,-1.02937753727333));
#4149=CARTESIAN_POINT('Ctrl Pts',(-1.85551383526763,4.05579201768493,-0.791671976409806));
#4150=CARTESIAN_POINT('Ctrl Pts',(-1.99633687991085,4.08540082780284,-0.286873759418399));
#4151=CARTESIAN_POINT('Ctrl Pts',(-2.01668239103348,4.09824266680982,-0.0251545927172321));
#4152=CARTESIAN_POINT('Ctrl Pts',(-1.95639182414602,4.12595008392364,0.488501251547938));
#4153=CARTESIAN_POINT('Ctrl Pts',(-1.87746515861466,4.1407380396657,0.735658527789376));
#4154=CARTESIAN_POINT('Ctrl Pts',(-1.62553284661629,4.17131294748868,1.19543155433835));
#4155=CARTESIAN_POINT('Ctrl Pts',(-1.45142503291765,4.18681224680635,1.40171692008769));
#4156=CARTESIAN_POINT('Ctrl Pts',(-1.04259593990855,4.21509773737192,1.72558683920426));
#4157=CARTESIAN_POINT('Ctrl Pts',(-0.815036462771399,4.22745620633834,1.84401178999322));
#4158=CARTESIAN_POINT('Ctrl Pts',(-0.385591264380167,4.2525071762445,1.9720265737401));
#4159=CARTESIAN_POINT('Ctrl Pts',(-0.193119675665181,4.26373468558621,2.));
#4160=CARTESIAN_POINT('Ctrl Pts',(4.78783679369599E-15,4.27500000000001,
2.));
#4161=CARTESIAN_POINT('Ctrl Pts',(-9.71445146547012E-16,4.36250000191184,
2.00000000000001));
#4162=CARTESIAN_POINT('Ctrl Pts',(-0.243975293587871,4.34826810978588,2.00000000000001));
#4163=CARTESIAN_POINT('Ctrl Pts',(-0.486052805080953,4.33414692161546,1.95535511648689));
#4164=CARTESIAN_POINT('Ctrl Pts',(-0.954650468971208,4.30681205788853,1.77620586455412));
#4165=CARTESIAN_POINT('Ctrl Pts',(-1.17505972947074,4.29434742704428,1.63875101545638));
#4166=CARTESIAN_POINT('Ctrl Pts',(-1.55739883696697,4.26519892138022,1.28250382752127));
#4167=CARTESIAN_POINT('Ctrl Pts',(-1.71351233898587,4.24965630570933,1.06497199965594));
#4168=CARTESIAN_POINT('Ctrl Pts',(-1.92769479020271,4.21945699872622,0.590839049257593));
#4169=CARTESIAN_POINT('Ctrl Pts',(-1.98729139697089,4.20506274456764,0.340314828621115));
#4170=CARTESIAN_POINT('Ctrl Pts',(-2.00954797662932,4.17808103015945,-0.180934760325271));
#4171=CARTESIAN_POINT('Ctrl Pts',(-1.9675919825813,4.16398096231088,-0.446845468523272));
#4172=CARTESIAN_POINT('Ctrl Pts',(-1.7834956004059,4.13358858419427,-0.942170436269723));
#4173=CARTESIAN_POINT('Ctrl Pts',(-1.6449810345462,4.11817556531004,-1.16729766358963));
#4174=CARTESIAN_POINT('Ctrl Pts',(-1.29487251259413,4.08887602700756,-1.54514285966028));
#4175=CARTESIAN_POINT('Ctrl Pts',(-1.08902820576111,4.07602664724791,-1.69650964028479));
#4176=CARTESIAN_POINT('Ctrl Pts',(-0.621006080495942,4.04872535660744,-1.91955540343306));
#4177=CARTESIAN_POINT('Ctrl Pts',(-0.361301926763335,4.03357594763971,-1.98488304645561));
#4178=CARTESIAN_POINT('Ctrl Pts',(0.162021093548409,4.00304877145485,-2.01015480855732));
#4179=CARTESIAN_POINT('Ctrl Pts',(0.420517058828189,3.98796984014687,-1.97234939629171));
#4180=CARTESIAN_POINT('Ctrl Pts',(0.906166143150877,3.95964031022804,-1.80123236434251));
#4181=CARTESIAN_POINT('Ctrl Pts',(1.12906709225369,3.94729600477414,-1.67056385612915));
#4182=CARTESIAN_POINT('Ctrl Pts',(1.52091712445733,3.91844586292025,-1.32571387488676));
#4183=CARTESIAN_POINT('Ctrl Pts',(1.68349038929167,3.90290771385181,-1.1120000086205));
#4184=CARTESIAN_POINT('Ctrl Pts',(1.91114725778974,3.87255536647302,-0.64261710248446));
#4185=CARTESIAN_POINT('Ctrl Pts',(1.97760963120897,3.85801258071494,-0.393116670908036));
#4186=CARTESIAN_POINT('Ctrl Pts',(2.01343691144459,3.83076750771852,0.125511018469023));
#4187=CARTESIAN_POINT('Ctrl Pts',(1.97932244832764,3.81720080245072,0.389881750771629));
#4188=CARTESIAN_POINT('Ctrl Pts',(1.81078776901429,3.78707999692248,0.88881552875744));
#4189=CARTESIAN_POINT('Ctrl Pts',(1.67858452272334,3.77161503396507,1.11861482411685));
#4190=CARTESIAN_POINT('Ctrl Pts',(1.33901702364243,3.74208747590405,1.50705950322995));
#4191=CARTESIAN_POINT('Ctrl Pts',(1.13758132292479,3.72885891241579,1.66434621300729));
#4192=CARTESIAN_POINT('Ctrl Pts',(0.676205697517938,3.70194533426706,1.90080719990041));
#4193=CARTESIAN_POINT('Ctrl Pts',(0.418538303422225,3.68691473627814,1.97360121051258));
#4194=CARTESIAN_POINT('Ctrl Pts',(0.10284044210722,3.66849902770143,1.99801918799822));
#4195=CARTESIAN_POINT('Ctrl Pts',(0.051391973731045,3.66549786704615,2.));
#4196=CARTESIAN_POINT('Ctrl Pts',(7.41933818794109E-16,3.66250000191184,
2.));
#4197=CARTESIAN_POINT('Origin',(0.,70.,0.));
#4198=CARTESIAN_POINT('',(1.66219536719514E-14,2.87500000000001,2.));
#4199=CARTESIAN_POINT('',(2.61585959811339E-14,2.96250000191184,2.));
#4200=CARTESIAN_POINT('',(-2.44929359829471E-16,70.,2.));
#4201=CARTESIAN_POINT('Ctrl Pts',(-2.67147415300428E-15,2.87500000000001,
2.));
#4202=CARTESIAN_POINT('Ctrl Pts',(0.142854417545159,2.88333317435681,2.));
#4203=CARTESIAN_POINT('Ctrl Pts',(0.285642418419913,2.89166247440784,1.98469424875995));
#4204=CARTESIAN_POINT('Ctrl Pts',(0.682597198502697,2.91481816991267,1.89818103146292));
#4205=CARTESIAN_POINT('Ctrl Pts',(0.925716172957715,2.92812717302022,1.79221826774021));
#4206=CARTESIAN_POINT('Ctrl Pts',(1.35184472923469,2.9555174173453,1.49605747809885));
#4207=CARTESIAN_POINT('Ctrl Pts',(1.53218851063789,2.97013947289794,1.31073737308708));
#4208=CARTESIAN_POINT('Ctrl Pts',(1.81863070732071,3.00056835732941,0.873779151272685));
#4209=CARTESIAN_POINT('Ctrl Pts',(1.91869602817475,3.01609874159016,0.6241300100535));
#4210=CARTESIAN_POINT('Ctrl Pts',(2.01318760980476,3.04477733779127,0.110995770600117));
#4211=CARTESIAN_POINT('Ctrl Pts',(2.01090097070637,3.05709343668879,-0.14670730974588));
#4212=CARTESIAN_POINT('Ctrl Pts',(1.90872769732121,3.08555539239449,-0.651118152739248));
#4213=CARTESIAN_POINT('Ctrl Pts',(1.80836309406561,3.10068935707265,-0.892747430518395));
#4214=CARTESIAN_POINT('Ctrl Pts',(1.51777575078367,3.13121115556886,-1.32915167232376));
#4215=CARTESIAN_POINT('Ctrl Pts',(1.32839168621177,3.14629813498382,-1.51845547314241));
#4216=CARTESIAN_POINT('Ctrl Pts',(0.896730869869025,3.17339142956617,-1.80554413046886));
#4217=CARTESIAN_POINT('Ctrl Pts',(0.661159371273239,3.18643237000908,-1.90447594325186));
#4218=CARTESIAN_POINT('Ctrl Pts',(0.156768122434926,3.21585519285798,-2.0110156257623));
#4219=CARTESIAN_POINT('Ctrl Pts',(-0.107961243487111,3.23129773920343,-2.01422501025046));
#4220=CARTESIAN_POINT('Ctrl Pts',(-0.626497303349286,3.26154567602872,-1.91776934607945));
#4221=CARTESIAN_POINT('Ctrl Pts',(-0.874929158688982,3.27534818132766,-1.81790614058459));
#4222=CARTESIAN_POINT('Ctrl Pts',(-1.31037026177602,3.30247174333069,-1.53240089327968));
#4223=CARTESIAN_POINT('Ctrl Pts',(-1.49523945497418,3.31694671969792,-1.35260494880721));
#4224=CARTESIAN_POINT('Ctrl Pts',(-1.79298548980222,3.34723065175449,-0.925042313880283));
#4225=CARTESIAN_POINT('Ctrl Pts',(-1.89983272617656,3.36277236045616,-0.679084547617561));
#4226=CARTESIAN_POINT('Ctrl Pts',(-2.00935353942889,3.39176223073334,-0.168465810346163));
#4227=CARTESIAN_POINT('Ctrl Pts',(-2.01437192448993,3.40415129531614,0.0904719705272669));
#4228=CARTESIAN_POINT('Ctrl Pts',(-1.92593105442421,3.43237101196896,0.598016130591884));
#4229=CARTESIAN_POINT('Ctrl Pts',(-1.83259363071763,3.44740231043446,0.841670288414954));
#4230=CARTESIAN_POINT('Ctrl Pts',(-1.55486165485373,3.47792829465682,1.2855794359492));
#4231=CARTESIAN_POINT('Ctrl Pts',(-1.37089308146782,3.49312607037783,1.48020307013478));
#4232=CARTESIAN_POINT('Ctrl Pts',(-0.947425565242967,3.5205961769955,1.77948107537659));
#4233=CARTESIAN_POINT('Ctrl Pts',(-0.714674206606716,3.53331067128129,1.88505586375424));
#4234=CARTESIAN_POINT('Ctrl Pts',(-0.314624656407887,3.55664689504289,1.98141733522263));
#4235=CARTESIAN_POINT('Ctrl Pts',(-0.15740419443768,3.56581808865781,2.));
#4236=CARTESIAN_POINT('Ctrl Pts',(1.38777878078145E-15,3.57500000000001,
2.));
#4237=CARTESIAN_POINT('Ctrl Pts',(1.62717062046625E-14,3.66250000191184,
2.));
#4238=CARTESIAN_POINT('Ctrl Pts',(-0.207355900358025,3.65040424105762,2.));
#4239=CARTESIAN_POINT('Ctrl Pts',(-0.413792093728005,3.63836212977771,1.96775009577714));
#4240=CARTESIAN_POINT('Ctrl Pts',(-0.854549734069061,3.61265126742448,1.82612830148329));
#4241=CARTESIAN_POINT('Ctrl Pts',(-1.08008775545534,3.60033644823094,1.70247079478363));
#4242=CARTESIAN_POINT('Ctrl Pts',(-1.4816897339598,3.57180552160872,1.36956992521774));
#4243=CARTESIAN_POINT('Ctrl Pts',(-1.65089053657749,3.55628470367144,1.1600255371002));
#4244=CARTESIAN_POINT('Ctrl Pts',(-1.89246080795477,3.52579628244731,0.695981974276634));
#4245=CARTESIAN_POINT('Ctrl Pts',(-1.9660518643494,3.51110938596556,0.44774463721724));
#4246=CARTESIAN_POINT('Ctrl Pts',(-2.0158918157091,3.48359753615755,-0.0680736440507168));
#4247=CARTESIAN_POINT('Ctrl Pts',(-1.98971941010455,3.47048355845382,-0.330902723038247));
#4248=CARTESIAN_POINT('Ctrl Pts',(-1.83711373268955,3.44065274920631,-0.833292676932479));
#4249=CARTESIAN_POINT('Ctrl Pts',(-1.71153971309772,3.42514819400045,-1.06770308137849));
#4250=CARTESIAN_POINT('Ctrl Pts',(-1.38290885522477,3.39539377052543,-1.46695280379187));
#4251=CARTESIAN_POINT('Ctrl Pts',(-1.18588972314158,3.38167690242843,-1.63032726093278));
#4252=CARTESIAN_POINT('Ctrl Pts',(-0.731360668453417,3.35516270757162,-1.88026878965662));
#4253=CARTESIAN_POINT('Ctrl Pts',(-0.475973639380006,3.34026513087567,-1.96053509495005));
#4254=CARTESIAN_POINT('Ctrl Pts',(0.0463498516951409,3.30979626056296,-2.01632879391251));
#4255=CARTESIAN_POINT('Ctrl Pts',(0.30806663221086,3.29452944836621,-1.99319836390888));
#4256=CARTESIAN_POINT('Ctrl Pts',(0.802029459668345,3.26571495009785,-1.84968137667425));
#4257=CARTESIAN_POINT('Ctrl Pts',(1.03025639010877,3.25332989512491,-1.7329555238452));
#4258=CARTESIAN_POINT('Ctrl Pts',(1.44142228330395,3.22512539488095,-1.41203794953861));
#4259=CARTESIAN_POINT('Ctrl Pts',(1.61711480830446,3.20963467736261,-1.20683739285706));
#4260=CARTESIAN_POINT('Ctrl Pts',(1.87240490201655,3.17903451791594,-0.74850312996786));
#4261=CARTESIAN_POINT('Ctrl Pts',(1.95306549537904,3.16421498493323,-0.501721870167323));
#4262=CARTESIAN_POINT('Ctrl Pts',(2.01674725741211,3.13644472993755,0.0112199341423071));
#4263=CARTESIAN_POINT('Ctrl Pts',(1.9982757761014,3.12367911104514,0.272587206719206));
#4264=CARTESIAN_POINT('Ctrl Pts',(1.86125774248558,3.09414330988512,0.7781370452862));
#4265=CARTESIAN_POINT('Ctrl Pts',(1.74232935182834,3.07861345336577,1.0168851415062));
#4266=CARTESIAN_POINT('Ctrl Pts',(1.42466403861883,3.04865399292359,1.42652450344923));
#4267=CARTESIAN_POINT('Ctrl Pts',(1.23194233115013,3.0344746889772,1.59593400063326));
#4268=CARTESIAN_POINT('Ctrl Pts',(0.784116556100397,3.00813043731828,1.85886261012239));
#4269=CARTESIAN_POINT('Ctrl Pts',(0.531122256623746,2.99348213354822,1.94633773788873));
#4270=CARTESIAN_POINT('Ctrl Pts',(0.179209454759298,2.9729538867728,1.99398432590961));
#4271=CARTESIAN_POINT('Ctrl Pts',(0.0895606200734576,2.96772437141612,2.));
#4272=CARTESIAN_POINT('Ctrl Pts',(7.41933818794109E-16,2.96250000191184,
2.));
#4273=CARTESIAN_POINT('Origin',(0.,70.,0.));
#4274=CARTESIAN_POINT('',(2.71387147450608E-14,2.17500000000001,2.));
#4275=CARTESIAN_POINT('',(2.37375725299738E-14,2.26250000191184,2.));
#4276=CARTESIAN_POINT('',(-2.44929359829471E-16,70.,2.));
#4277=CARTESIAN_POINT('Ctrl Pts',(1.35655375821386E-14,2.17500000000001,
2.));
#4278=CARTESIAN_POINT('Ctrl Pts',(0.182979636269589,2.18567381211573,2.));
#4279=CARTESIAN_POINT('Ctrl Pts',(0.365491336649497,2.19632032797123,1.97488723208934));
#4280=CARTESIAN_POINT('Ctrl Pts',(0.791337489295804,2.22116135354227,1.85491186723268));
#4281=CARTESIAN_POINT('Ctrl Pts',(1.02430206525457,2.23378427945719,1.73715519322295));
#4282=CARTESIAN_POINT('Ctrl Pts',(1.43173051123552,2.26168749328194,1.42004372716924));
#4283=CARTESIAN_POINT('Ctrl Pts',(1.60253840374314,2.27657231975359,1.22401655890837));
#4284=CARTESIAN_POINT('Ctrl Pts',(1.86551616881027,2.3072216491371,0.769147462816087));
#4285=CARTESIAN_POINT('Ctrl Pts',(1.95165471009802,2.32269142931126,0.512657341461188));
#4286=CARTESIAN_POINT('Ctrl Pts',(2.01602776099352,2.35072106227596,-0.00501969927426783));
#4287=CARTESIAN_POINT('Ctrl Pts',(1.99914036922866,2.36318353242911,-0.26046995469053));
#4288=CARTESIAN_POINT('Ctrl Pts',(1.86898493410317,2.3921232774136,-0.758183063998182));
#4289=CARTESIAN_POINT('Ctrl Pts',(1.7543702215466,2.40743215030844,-0.995047322113318));
#4290=CARTESIAN_POINT('Ctrl Pts',(1.43812396380874,2.43786779255932,-1.4149319313869));
#4291=CARTESIAN_POINT('Ctrl Pts',(1.23815836053804,2.45268945480269,-1.59287456003142));
#4292=CARTESIAN_POINT('Ctrl Pts',(0.790103953079335,2.47898836731802,-1.85477368624924));
#4293=CARTESIAN_POINT('Ctrl Pts',(0.548432060457288,2.49300812980667,-1.94004603316793));
#4294=CARTESIAN_POINT('Ctrl Pts',(0.0363177609825734,2.5228814639427,-2.01699349355232));
#4295=CARTESIAN_POINT('Ctrl Pts',(-0.229740885380059,2.53840155164718,-2.00419789204612));
#4296=CARTESIAN_POINT('Ctrl Pts',(-0.738375400475203,2.56807189836107,-1.87687947883354));
#4297=CARTESIAN_POINT('Ctrl Pts',(-0.976262444410051,2.58098300576251,-1.76487034365478));
#4298=CARTESIAN_POINT('Ctrl Pts',(-1.39291398846778,2.60863690599144,-1.45801896507246));
#4299=CARTESIAN_POINT('Ctrl Pts',(-1.56849735241706,2.62339761807215,-1.26720574431744));
#4300=CARTESIAN_POINT('Ctrl Pts',(-1.84316960403584,2.65395003042836,-0.821006922788507));
#4301=CARTESIAN_POINT('Ctrl Pts',(-1.9362248745901,2.66945599004052,-0.56779400979672));
#4302=CARTESIAN_POINT('Ctrl Pts',(-2.0154427085729,2.69780963370476,-0.0522738600723176));
#4303=CARTESIAN_POINT('Ctrl Pts',(-2.00574981824586,2.71015036433805,0.204244764812837));
#4304=CARTESIAN_POINT('Ctrl Pts',(-1.88946498189406,2.73885605799548,0.705333053313018));
#4305=CARTESIAN_POINT('Ctrl Pts',(-1.7818984055525,2.75408407701296,0.944666063070827));
#4306=CARTESIAN_POINT('Ctrl Pts',(-1.47827330814531,2.78457551452497,1.37294196239716));
#4307=CARTESIAN_POINT('Ctrl Pts',(-1.28347335848784,2.79953528661918,1.55660084858788));
#4308=CARTESIAN_POINT('Ctrl Pts',(-0.843495908200234,2.82623234117405,1.83104437667243));
#4309=CARTESIAN_POINT('Ctrl Pts',(-0.604909818686825,2.83971359390995,1.9231130425793));
#4310=CARTESIAN_POINT('Ctrl Pts',(-0.237846563856373,2.86112561710839,1.98939716012295));
#4311=CARTESIAN_POINT('Ctrl Pts',(-0.118900276756154,2.86806415052256,2.));
#4312=CARTESIAN_POINT('Ctrl Pts',(-1.56472057533108E-14,2.87500000000001,
2.));
#4313=CARTESIAN_POINT('Ctrl Pts',(-1.870031907103E-14,2.96250000191184,
2.));
#4314=CARTESIAN_POINT('Ctrl Pts',(-0.170295006100021,2.95256612655601,2.));
#4315=CARTESIAN_POINT('Ctrl Pts',(-0.340271071332373,2.94265085608412,1.97824864775472));
#4316=CARTESIAN_POINT('Ctrl Pts',(-0.751083640266264,2.91868678956298,1.87087579921638));
#4317=CARTESIAN_POINT('Ctrl Pts',(-0.98193900049545,2.90614098403221,1.76070459522563));
#4318=CARTESIAN_POINT('Ctrl Pts',(-1.39965977067423,2.87841458049973,1.45303534142691));
#4319=CARTESIAN_POINT('Ctrl Pts',(-1.5797910577715,2.86314747147452,1.25482380547795));
#4320=CARTESIAN_POINT('Ctrl Pts',(-1.84851543059949,2.83263313129627,0.8059446082032));
#4321=CARTESIAN_POINT('Ctrl Pts',(-1.93697072901004,2.81767938203182,0.561006830098362));
#4322=CARTESIAN_POINT('Ctrl Pts',(-2.01587940205785,2.78963075638733,0.0513459771668947));
#4323=CARTESIAN_POINT('Ctrl Pts',(-2.00572725273602,2.77713418851999,-0.208496521839839));
#4324=CARTESIAN_POINT('Ctrl Pts',(-1.88567989006105,2.74793159773073,-0.717248527079829));
#4325=CARTESIAN_POINT('Ctrl Pts',(-1.77415593218552,2.7323894605413,-0.96051466878277));
#4326=CARTESIAN_POINT('Ctrl Pts',(-1.46866489711293,2.70222075332442,-1.3813248654293));
#4327=CARTESIAN_POINT('Ctrl Pts',(-1.28072316225833,2.6878549600921,-1.5571856115837));
#4328=CARTESIAN_POINT('Ctrl Pts',(-0.83876688931226,2.6609226030884,-1.83514444640525));
#4329=CARTESIAN_POINT('Ctrl Pts',(-0.586517626705013,2.6467135301363,-1.93063622781826));
#4330=CARTESIAN_POINT('Ctrl Pts',(-0.0646611294151879,2.61627190112773,
-2.01600742742588));
#4331=CARTESIAN_POINT('Ctrl Pts',(0.199371655450169,2.60086998867725,-2.00716806135491));
#4332=CARTESIAN_POINT('Ctrl Pts',(0.700909854133423,2.57161359375406,-1.89021092239354));
#4333=CARTESIAN_POINT('Ctrl Pts',(0.934382523524579,2.55882394907885,-1.78635678502449));
#4334=CARTESIAN_POINT('Ctrl Pts',(1.35998525898409,2.53145074879445,-1.49022979710036));
#4335=CARTESIAN_POINT('Ctrl Pts',(1.54537189209187,2.51628048076993,-1.29696939125311));
#4336=CARTESIAN_POINT('Ctrl Pts',(1.82645344292305,2.48575319485243,-0.854968354846357));
#4337=CARTESIAN_POINT('Ctrl Pts',(1.9216149980674,2.47069422434185,-0.611819595365497));
#4338=CARTESIAN_POINT('Ctrl Pts',(2.01361840955679,2.4424111985188,-0.105079072986001));
#4339=CARTESIAN_POINT('Ctrl Pts',(2.01050509035082,2.43005029389354,0.153531091476245));
#4340=CARTESIAN_POINT('Ctrl Pts',(1.90489887199435,2.40114067312447,0.664821392875117));
#4341=CARTESIAN_POINT('Ctrl Pts',(1.79980646867443,2.3856006996941,0.911757963010447));
#4342=CARTESIAN_POINT('Ctrl Pts',(1.50497723934194,2.35527678943077,1.34179597963616));
#4343=CARTESIAN_POINT('Ctrl Pts',(1.32127121823364,2.34076249986297,1.52304168137978));
#4344=CARTESIAN_POINT('Ctrl Pts',(0.888254477253353,2.31356877136604,1.81133557117034));
#4345=CARTESIAN_POINT('Ctrl Pts',(0.641222071284661,2.29990462273678,1.91280290869273));
#4346=CARTESIAN_POINT('Ctrl Pts',(0.2555299886456,2.27740591791616,1.98775831208609));
#4347=CARTESIAN_POINT('Ctrl Pts',(0.127758721976142,2.26995259402711,2.));
#4348=CARTESIAN_POINT('Ctrl Pts',(1.68615121864946E-14,2.26250000191184,
2.));
#4349=CARTESIAN_POINT('Origin',(0.,70.,0.));
#4350=CARTESIAN_POINT('',(-3.85812841423205E-14,1.475,2.));
#4351=CARTESIAN_POINT('',(3.55434499861684E-14,1.56250000191184,2.));
#4352=CARTESIAN_POINT('',(-2.44929359829471E-16,70.,2.));
#4353=CARTESIAN_POINT('Ctrl Pts',(-1.4210854715202E-13,1.475,2.));
#4354=CARTESIAN_POINT('Ctrl Pts',(0.223954565798372,1.48806401633825,2.00000000000002));
#4355=CARTESIAN_POINT('Ctrl Pts',(0.446651237620323,1.50105465552787,1.9623799948505));
#4356=CARTESIAN_POINT('Ctrl Pts',(0.900089169467497,1.52750520155229,1.80421749486211));
#4357=CARTESIAN_POINT('Ctrl Pts',(1.12307065137741,1.53982838655968,1.67453697057544));
#4358=CARTESIAN_POINT('Ctrl Pts',(1.51076243853498,1.56824166311884,1.33593391556795));
#4359=CARTESIAN_POINT('Ctrl Pts',(1.67091754054934,1.58335571929184,1.12921878454133));
#4360=CARTESIAN_POINT('Ctrl Pts',(1.90620009350724,1.61388037620501,0.660827725173358));
#4361=CARTESIAN_POINT('Ctrl Pts',(1.9769374846594,1.62899082464268,0.402558669348879));
#4362=CARTESIAN_POINT('Ctrl Pts',(2.01270379504195,1.65616111587045,-0.114623925871697));
#4363=CARTESIAN_POINT('Ctrl Pts',(1.98205222019211,1.66912791403358,-0.368272346770132));
#4364=CARTESIAN_POINT('Ctrl Pts',(1.82499297610609,1.69850535884176,-0.859116744253398));
#4365=CARTESIAN_POINT('Ctrl Pts',(1.6968392350588,1.71393742373891,-1.09060280984857));
#4366=CARTESIAN_POINT('Ctrl Pts',(1.35620729238248,1.74423917115757,-1.49375790704674));
#4367=CARTESIAN_POINT('Ctrl Pts',(1.14602139104281,1.75814875218919,-1.66047779684889));
#4368=CARTESIAN_POINT('Ctrl Pts',(0.68194353692421,1.78521996034611,-1.89742151731383));
#4369=CARTESIAN_POINT('Ctrl Pts',(0.434308572257149,1.79966533328502,-1.96890560133894));
#4370=CARTESIAN_POINT('Ctrl Pts',(-0.0843191117818514,1.82991861485396,
-2.01576595793462));
#4371=CARTESIAN_POINT('Ctrl Pts',(-0.350761000175043,1.84546105834356,-1.98680844766632));
#4372=CARTESIAN_POINT('Ctrl Pts',(-0.84874346307474,1.87451003534605,-1.82911354044634));
#4373=CARTESIAN_POINT('Ctrl Pts',(-1.07641941754803,1.88692413493962,-1.70509214089635));
#4374=CARTESIAN_POINT('Ctrl Pts',(-1.4735737909184,1.91509679720116,-1.37671524045494));
#4375=CARTESIAN_POINT('Ctrl Pts',(-1.6389065717559,1.930107164216,-1.17504195672059));
#4376=CARTESIAN_POINT('Ctrl Pts',(-1.88692619873131,1.9606311148776,-0.714018630620639));
#4377=CARTESIAN_POINT('Ctrl Pts',(-1.96488487202629,1.97584868051013,-0.457798413426827));
#4378=CARTESIAN_POINT('Ctrl Pts',(-2.01513953465624,2.0033900823559,0.0583654128161219));
#4379=CARTESIAN_POINT('Ctrl Pts',(-1.99156021339034,2.01605324342356,0.3128990953386));
#4380=CARTESIAN_POINT('Ctrl Pts',(-1.84837802151728,2.04520766626291,0.807340722581691));
#4381=CARTESIAN_POINT('Ctrl Pts',(-1.72718253099971,2.06058178955858,1.04169718973461));
#4382=CARTESIAN_POINT('Ctrl Pts',(-1.39912001823063,2.09095620884004,1.45354778048657));
#4383=CARTESIAN_POINT('Ctrl Pts',(-1.19431701439985,2.10533150749335,1.62599281106236));
#4384=CARTESIAN_POINT('Ctrl Pts',(-0.738641153368917,2.13191259938682,1.87597514462229));
#4385=CARTESIAN_POINT('Ctrl Pts',(-0.494017521167705,2.14618231126523,1.95468012692659));
#4386=CARTESIAN_POINT('Ctrl Pts',(-0.16104599383136,2.16560565035985,1.99514263757503));
#4387=CARTESIAN_POINT('Ctrl Pts',(-0.0804777381855486,2.17030546527252,
2.));
#4388=CARTESIAN_POINT('Ctrl Pts',(7.06522986662669E-16,2.17500000000001,
2.));
#4389=CARTESIAN_POINT('Ctrl Pts',(8.91647866652079E-15,2.26250000191184,
2.));
#4390=CARTESIAN_POINT('Ctrl Pts',(-0.133416331800623,2.2547173825568,2.));
#4391=CARTESIAN_POINT('Ctrl Pts',(-0.266818983260238,2.24693556122166,1.98665001605873));
#4392=CARTESIAN_POINT('Ctrl Pts',(-0.646448707316979,2.22479049398501,1.90952359766146));
#4393=CARTESIAN_POINT('Ctrl Pts',(-0.882803305241684,2.2116438631352,1.8123973313908));
#4394=CARTESIAN_POINT('Ctrl Pts',(-1.31666706932481,2.18465417488529,1.52863142004111));
#4395=CARTESIAN_POINT('Ctrl Pts',(-1.50749435171128,2.16959942830896,1.34079890614957));
#4396=CARTESIAN_POINT('Ctrl Pts',(-1.80153755051224,2.13908306064985,0.90649740615324));
#4397=CARTESIAN_POINT('Ctrl Pts',(-1.90380360717819,2.1239231559428,0.665452453606646));
#4398=CARTESIAN_POINT('Ctrl Pts',(-2.00969796320355,2.09539638641008,0.161906997632573));
#4399=CARTESIAN_POINT('Ctrl Pts',(-2.01394684785679,2.08308360048019,-0.0954742925500754));
#4400=CARTESIAN_POINT('Ctrl Pts',(-1.92349946949502,2.05449019122032,-0.609257189730553));
#4401=CARTESIAN_POINT('Ctrl Pts',(-1.82527917470336,2.0389650075537,-0.859868612177484));
#4402=CARTESIAN_POINT('Ctrl Pts',(-1.54192651951901,2.00850107238417,-1.29930440628386));
#4403=CARTESIAN_POINT('Ctrl Pts',(-1.36282768343608,1.9938412321369,-1.48609122379259));
#4404=CARTESIAN_POINT('Ctrl Pts',(-0.939207245649434,1.96638046159267,-1.78509613340325));
#4405=CARTESIAN_POINT('Ctrl Pts',(-0.697490100720316,1.95318692445385,-1.89267404339112));
#4406=CARTESIAN_POINT('Ctrl Pts',(-0.185133210869436,1.92329943921255,-2.00873304752374));
#4407=CARTESIAN_POINT('Ctrl Pts',(0.0805470681854508,1.90780142293435,-2.0156364878012));
#4408=CARTESIAN_POINT('Ctrl Pts',(0.589884203102323,1.8780900900642,-1.92779010209547));
#4409=CARTESIAN_POINT('Ctrl Pts',(0.829285228352145,1.864474850519,-1.837537672256));
#4410=CARTESIAN_POINT('Ctrl Pts',(1.27143703921337,1.83788368417352,-1.56644555478925));
#4411=CARTESIAN_POINT('Ctrl Pts',(1.4676374048311,1.82295966690869,-1.38430296119986));
#4412=CARTESIAN_POINT('Ctrl Pts',(1.77466543106788,1.79248065499219,-0.958237706752163));
#4413=CARTESIAN_POINT('Ctrl Pts',(1.8841247533492,1.77722982458753,-0.719545926011083));
#4414=CARTESIAN_POINT('Ctrl Pts',(2.00412757277745,1.74846085058755,-0.219351590116043));
#4415=CARTESIAN_POINT('Ctrl Pts',(2.01575665841001,1.7360969016035,0.0368712940846499));
#4416=CARTESIAN_POINT('Ctrl Pts',(1.94053433806999,1.70782968876513,0.552987368037824));
#4417=CARTESIAN_POINT('Ctrl Pts',(1.84933110419448,1.69233226331264,0.807100622354414));
#4418=CARTESIAN_POINT('Ctrl Pts',(1.57778244929932,1.66175151715696,1.25566371706682));
#4419=CARTESIAN_POINT('Ctrl Pts',(1.40347029545737,1.64695635989922,1.4478927089961));
#4420=CARTESIAN_POINT('Ctrl Pts',(0.989299965515635,1.61923469029751,1.75751810289436));
#4421=CARTESIAN_POINT('Ctrl Pts',(0.752753555657878,1.60641062599187,1.87108596660523));
#4422=CARTESIAN_POINT('Ctrl Pts',(0.337028356974093,1.58215998940198,1.97866476993144));
#4423=CARTESIAN_POINT('Ctrl Pts',(0.168658385814324,1.57233840775101,2.));
#4424=CARTESIAN_POINT('Ctrl Pts',(4.85722573273506E-16,1.56250000191184,
2.));
#4425=CARTESIAN_POINT('Origin',(0.,70.,0.));
#4426=CARTESIAN_POINT('',(-7.54708115709547E-15,0.775000000000007,2.));
#4427=CARTESIAN_POINT('',(2.64014572677706E-14,0.862500001911841,2.));
#4428=CARTESIAN_POINT('',(-2.44929359829471E-16,70.,2.));
#4429=CARTESIAN_POINT('Ctrl Pts',(-1.38777878078145E-15,0.775000000000008,
2.));
#4430=CARTESIAN_POINT('Ctrl Pts',(0.263641812514793,0.790379105730038,2.));
#4431=CARTESIAN_POINT('Ctrl Pts',(0.524773806618217,0.805611805386091,1.94786890290239));
#4432=CARTESIAN_POINT('Ctrl Pts',(1.00270510760052,0.833491131276723,1.7490090237614));
#4433=CARTESIAN_POINT('Ctrl Pts',(1.2163618842073,0.845922301161266,1.60777046374085));
#4434=CARTESIAN_POINT('Ctrl Pts',(1.58424989383885,0.874816756963846,1.2482088136233));
#4435=CARTESIAN_POINT('Ctrl Pts',(1.73319192739454,0.890110749075232,1.0314580066477));
#4436=CARTESIAN_POINT('Ctrl Pts',(1.94137076405355,0.920559320787235,0.548924705768364));
#4437=CARTESIAN_POINT('Ctrl Pts',(1.9969671379211,0.935408976994167,0.287076326897205));
#4438=CARTESIAN_POINT('Ctrl Pts',(2.00266664909294,0.961786339306387,-0.231769421015456));
#4439=CARTESIAN_POINT('Ctrl Pts',(1.95713900686814,0.975692568602954,-0.483835156331504));
#4440=CARTESIAN_POINT('Ctrl Pts',(1.77062477881778,1.00552284657222,-0.966637482806648));
#4441=CARTESIAN_POINT('Ctrl Pts',(1.62792865993129,1.02103774381255,-1.19136715780624));
#4442=CARTESIAN_POINT('Ctrl Pts',(1.26545504715454,1.05076689279692,-1.57057745140074));
#4443=CARTESIAN_POINT('Ctrl Pts',(1.05002459454285,1.06374856531836,-1.7220676167783));
#4444=CARTESIAN_POINT('Ctrl Pts',(0.576842766048914,1.09135083864717,-1.93215175399565));
#4445=CARTESIAN_POINT('Ctrl Pts',(0.324257631581426,1.10608497149111,-1.99017081615757));
#4446=CARTESIAN_POINT('Ctrl Pts',(-0.199111495671019,1.1366148372475,-2.00788391891833));
#4447=CARTESIAN_POINT('Ctrl Pts',(-0.465028558889729,1.15212666593526,-1.96342070884061));
#4448=CARTESIAN_POINT('Ctrl Pts',(-0.952205920019837,1.18054534533451,-1.77711387884304));
#4449=CARTESIAN_POINT('Ctrl Pts',(-1.17044128448817,1.19287314868519,-1.641615758944));
#4450=CARTESIAN_POINT('Ctrl Pts',(-1.54823753074778,1.22153080742898,-1.29246199804695));
#4451=CARTESIAN_POINT('Ctrl Pts',(-1.7028485139701,1.2367410570788,-1.0806418315239));
#4452=CARTESIAN_POINT('Ctrl Pts',(-1.92465185066364,1.26724065016377,-0.604964678147023));
#4453=CARTESIAN_POINT('Ctrl Pts',(-1.98782202608,1.2822267987879,-0.344787186479645));
#4454=CARTESIAN_POINT('Ctrl Pts',(-2.0085179530319,1.30900338630977,0.173302986422976));
#4455=CARTESIAN_POINT('Ctrl Pts',(-1.97044884668927,1.32238847684033,0.4261155410126));
#4456=CARTESIAN_POINT('Ctrl Pts',(-1.79873862119006,1.35199476629224,0.913031139575736));
#4457=CARTESIAN_POINT('Ctrl Pts',(-1.66330887508614,1.36747489263217,1.14126777153031));
#4458=CARTESIAN_POINT('Ctrl Pts',(-1.3116979731138,1.39749737524703,1.5325561541498));
#4459=CARTESIAN_POINT('Ctrl Pts',(-1.09889701745739,1.41089767398167,1.69164661172676));
#4460=CARTESIAN_POINT('Ctrl Pts',(-0.630261499474268,1.43823474586402,1.91529946453159));
#4461=CARTESIAN_POINT('Ctrl Pts',(-0.380091506104799,1.45282799547724,1.98017506043044));
#4462=CARTESIAN_POINT('Ctrl Pts',(-0.0830206559478754,1.47015712840306,
1.99870903416013));
#4463=CARTESIAN_POINT('Ctrl Pts',(-0.0414887428399634,1.47257982333434,
2.));
#4464=CARTESIAN_POINT('Ctrl Pts',(-1.50526581573235E-13,1.475,2.));
#4465=CARTESIAN_POINT('Ctrl Pts',(7.41933818794109E-16,1.56250000191184,
2.));
#4466=CARTESIAN_POINT('Ctrl Pts',(-0.0941640936003199,1.55700709645182,
2.));
#4467=CARTESIAN_POINT('Ctrl Pts',(-0.188418089770249,1.55150894667523,1.99335001499073));
#4468=CARTESIAN_POINT('Ctrl Pts',(-0.533623864488207,1.53137194315001,1.94417515988776));
#4469=CARTESIAN_POINT('Ctrl Pts',(-0.776121134681528,1.5172262690554,1.86071371261903));
#4470=CARTESIAN_POINT('Ctrl Pts',(-1.22623678899418,1.49096952255383,1.60204214273226));
#4471=CARTESIAN_POINT('Ctrl Pts',(-1.42755153341047,1.47621646136407,1.42562718359061));
#4472=CARTESIAN_POINT('Ctrl Pts',(-1.74709544586349,1.44578927622245,1.00781388350229));
#4473=CARTESIAN_POINT('Ctrl Pts',(-1.8635057748182,1.43046160716481,0.771614257467079));
#4474=CARTESIAN_POINT('Ctrl Pts',(-1.99720748551615,1.40146292080669,0.274781854700861));
#4475=CARTESIAN_POINT('Ctrl Pts',(-2.01592235701723,1.38895402525217,0.019589420613992));
#4476=CARTESIAN_POINT('Ctrl Pts',(-1.95564851891177,1.36116039250832,-0.495782708893493));
#4477=CARTESIAN_POINT('Ctrl Pts',(-1.87273279584763,1.34587593916101,-0.750465005444869));
#4478=CARTESIAN_POINT('Ctrl Pts',(-1.61604197277987,1.31536666819081,-1.20619143161691));
#4479=CARTESIAN_POINT('Ctrl Pts',(-1.44721963392012,1.3004343306366,-1.40430543534141));
#4480=CARTESIAN_POINT('Ctrl Pts',(-1.04355166329762,1.27243148996314,-1.72556011301291));
#4481=CARTESIAN_POINT('Ctrl Pts',(-0.81254646348664,1.25989854561521,-1.84562551552966));
#4482=CARTESIAN_POINT('Ctrl Pts',(-0.310972319885067,1.23064005390512,-1.99335257263115));
#4483=CARTESIAN_POINT('Ctrl Pts',(-0.0445515678019491,1.21509884336694,
-2.01696751857633));
#4484=CARTESIAN_POINT('Ctrl Pts',(0.472067650418802,1.18496272230406,-1.96013306796473));
#4485=CARTESIAN_POINT('Ctrl Pts',(0.717825270595456,1.17062686112709,-1.88407560427836));
#4486=CARTESIAN_POINT('Ctrl Pts',(1.17863878906077,1.14374607254995,-1.6377962436916));
#4487=CARTESIAN_POINT('Ctrl Pts',(1.38695540224028,1.12942016937891,-1.4656059683808));
#4488=CARTESIAN_POINT('Ctrl Pts',(1.71966797178848,1.09892764261738,-1.05410216737661));
#4489=CARTESIAN_POINT('Ctrl Pts',(1.84262257064793,1.08353778589356,-0.82044988079058));
#4490=CARTESIAN_POINT('Ctrl Pts',(1.98930206580404,1.05432659707209,-0.326903747509112));
#4491=CARTESIAN_POINT('Ctrl Pts',(2.01466873925147,1.04159555592171,-0.0726019437903748));
#4492=CARTESIAN_POINT('Ctrl Pts',(1.96808522885465,1.01414748587772,0.443833932638237));
#4493=CARTESIAN_POINT('Ctrl Pts',(1.89195071824916,0.998955904156174,0.70059298260607));
#4494=CARTESIAN_POINT('Ctrl Pts',(1.64713688415654,0.968429476623535,1.16351620342109));
#4495=CARTESIAN_POINT('Ctrl Pts',(1.48310153656839,0.953391807058156,1.36647901093069));
#4496=CARTESIAN_POINT('Ctrl Pts',(1.08833999596802,0.925157628666796,1.69745511758567));
#4497=CARTESIAN_POINT('Ctrl Pts',(0.861866671489158,0.912775557748692,1.8229169881279));
#4498=CARTESIAN_POINT('Ctrl Pts',(0.417954610804559,0.886880687542087,1.96709817284442));
#4499=CARTESIAN_POINT('Ctrl Pts',(0.209440523454726,0.87471736578003,2.));
#4500=CARTESIAN_POINT('Ctrl Pts',(8.67361737988404E-16,0.862500001911838,
2.));
#4501=CARTESIAN_POINT('Origin',(0.,0.45,0.));
#4502=CARTESIAN_POINT('',(-2.44929359829471E-16,0.440000000000001,-2.));
#4503=CARTESIAN_POINT('',(1.90060369884293E-8,0.404509613602118,-1.96450961360212));
#4504=CARTESIAN_POINT('',(-2.46154006628618E-16,0.45,-2.01));
#4505=CARTESIAN_POINT('',(1.07566249295046,0.444996920070102,-1.69202921096245));
#4506=CARTESIAN_POINT('Origin',(0.,0.440000000000001,0.));
#4507=CARTESIAN_POINT('',(1.22721437665197,0.445850114232433,-1.58662519203873));
#4508=CARTESIAN_POINT('Ctrl Pts',(1.07566249295046,0.444996920070102,-1.69202921096245));
#4509=CARTESIAN_POINT('Ctrl Pts',(1.09611643683742,0.443060583023077,-1.67673166768133));
#4510=CARTESIAN_POINT('Ctrl Pts',(1.1167162602212,0.441907359466892,-1.66168928306883));
#4511=CARTESIAN_POINT('Ctrl Pts',(1.13725615399585,0.44160691752963,-1.64714258414414));
#4512=CARTESIAN_POINT('Ctrl Pts',(1.15842534493283,0.441297270712311,-1.63215020636371));
#4513=CARTESIAN_POINT('Ctrl Pts',(1.17953119574262,0.441893460704303,-1.61768416278773));
#4514=CARTESIAN_POINT('Ctrl Pts',(1.20038775671367,0.443471757258991,-1.60404747924317));
#4515=CARTESIAN_POINT('Ctrl Pts',(1.20941519791304,0.44415489861496,-1.59814505079277));
#4516=CARTESIAN_POINT('Ctrl Pts',(1.21839639510557,0.445022033500666,-1.59239850981534));
#4517=CARTESIAN_POINT('Ctrl Pts',(1.22731813304862,0.446079346610564,-1.58683475673666));
#4518=CARTESIAN_POINT('',(1.31150072492913E-11,0.264072050762771,1.82407205076277));
#4519=CARTESIAN_POINT('Ctrl Pts',(1.22456646636222,0.44,-1.5812770059231));
#4520=CARTESIAN_POINT('Ctrl Pts',(1.34092436486328,0.434825310204451,-1.48462261860236));
#4521=CARTESIAN_POINT('Ctrl Pts',(1.44576508331674,0.429407853078801,-1.37490110720192));
#4522=CARTESIAN_POINT('Ctrl Pts',(1.62424340516482,0.418528363271193,-1.13898239124983));
#4523=CARTESIAN_POINT('Ctrl Pts',(1.69851441965134,0.413111710208662,-1.01444043254867));
#4524=CARTESIAN_POINT('Ctrl Pts',(1.85949786400429,0.398560929406842,-0.661377198370944));
#4525=CARTESIAN_POINT('Ctrl Pts',(1.91858368406403,0.389540675297832,-0.423038305434833));
#4526=CARTESIAN_POINT('Ctrl Pts',(1.94755017248106,0.372319500206739,0.073807683981543));
#4527=CARTESIAN_POINT('Ctrl Pts',(1.91303291352136,0.363978840607724,0.326681990469294));
#4528=CARTESIAN_POINT('Ctrl Pts',(1.74862425848826,0.345324659582443,0.794041188679305));
#4529=CARTESIAN_POINT('Ctrl Pts',(1.62615811693947,0.335882829432591,1.00394140613174));
#4530=CARTESIAN_POINT('Ctrl Pts',(1.27814151888825,0.315411208564217,1.40228678216834));
#4531=CARTESIAN_POINT('Ctrl Pts',(1.06504837422352,0.306309114754379,1.54645068384557));
#4532=CARTESIAN_POINT('Ctrl Pts',(0.738669273324379,0.293563865877837,1.70724532485268));
#4533=CARTESIAN_POINT('Ctrl Pts',(0.589469481980592,0.287689020611286,1.75814842742425));
#4534=CARTESIAN_POINT('Ctrl Pts',(0.292319615601393,0.275866774827419,1.81832292184012));
#4535=CARTESIAN_POINT('Ctrl Pts',(0.146071997417127,0.269995076562265,1.82999507656121));
#4536=CARTESIAN_POINT('Ctrl Pts',(1.31614857901141E-11,0.264072050762774,
1.82407205076277));
#4537=CARTESIAN_POINT('',(-0.414966524668622,0.0611138874999821,-1.56710338511853));
#4538=CARTESIAN_POINT('Ctrl Pts',(1.31119073931707E-11,0.264072050762771,
1.82407205076277));
#4539=CARTESIAN_POINT('Ctrl Pts',(-0.182500618677702,0.256671892675391,
1.8166718926767));
#4540=CARTESIAN_POINT('Ctrl Pts',(-0.362846391412083,0.249266998949665,
1.7818819341821));
#4541=CARTESIAN_POINT('Ctrl Pts',(-0.695425892968101,0.235448646498967,
1.66401272030053));
#4542=CARTESIAN_POINT('Ctrl Pts',(-0.874684974565809,0.228481241516197,
1.57533708528328));
#4543=CARTESIAN_POINT('Ctrl Pts',(-1.22898394413066,0.211375383019265,1.29647398987752));
#4544=CARTESIAN_POINT('Ctrl Pts',(-1.38061231788004,0.201854495765184,1.11869581647509));
#4545=CARTESIAN_POINT('Ctrl Pts',(-1.60022755658981,0.182831136549121,0.724548107605763));
#4546=CARTESIAN_POINT('Ctrl Pts',(-1.67005790774639,0.173520054063588,0.514053964643143));
#4547=CARTESIAN_POINT('Ctrl Pts',(-1.71881409521262,0.158649088175912,0.147705584520746));
#4548=CARTESIAN_POINT('Ctrl Pts',(-1.73283633029671,0.150263481745077,-0.0918032208300236));
#4549=CARTESIAN_POINT('Ctrl Pts',(-1.60131282490526,0.129348630402047,-0.577463975714151));
#4550=CARTESIAN_POINT('Ctrl Pts',(-1.50916906144907,0.120153028228782,-0.767510573105503));
#4551=CARTESIAN_POINT('Ctrl Pts',(-1.26910066605646,0.102383574220385,-1.09098903228809));
#4552=CARTESIAN_POINT('Ctrl Pts',(-1.12774845722577,0.093949227674449,-1.22519616910076));
#4553=CARTESIAN_POINT('Ctrl Pts',(-0.822715308031425,0.0789309073211611,
-1.42794886846669));
#4554=CARTESIAN_POINT('Ctrl Pts',(-0.638864841828697,0.0712113726913205,
-1.51826095786994));
#4555=CARTESIAN_POINT('Ctrl Pts',(-0.41496652466861,0.0611138875000055,
-1.56710338511849));
#4556=CARTESIAN_POINT('',(-1.9852919333802E-16,0.061113887500004,-1.6211138875));
#4557=CARTESIAN_POINT('Origin',(-1.15733580648385E-15,0.0611138875000017,
-3.60822483003176E-15));
#4558=CARTESIAN_POINT('',(-1.91044900666986E-16,-2.08166817117217E-16,-1.55999999999999));
#4559=CARTESIAN_POINT('',(-2.46154006628618E-16,0.45,-2.01));
#4560=CARTESIAN_POINT('Origin',(0.,0.,0.));
#4561=CARTESIAN_POINT('',(1.55927926836488,0.0611138874999996,-0.443461835441161));
#4562=CARTESIAN_POINT('Origin',(-1.15733580648385E-15,0.0611138875000017,
-3.60822483003176E-15));
#4563=CARTESIAN_POINT('Ctrl Pts',(1.55927926836487,0.0611138874999902,-0.443461835441164));
#4564=CARTESIAN_POINT('Ctrl Pts',(1.54461788344873,0.0822167370265837,-0.572156824316265));
#4565=CARTESIAN_POINT('Ctrl Pts',(1.51500223189783,0.103443446107898,-0.698682493147245));
#4566=CARTESIAN_POINT('Ctrl Pts',(1.4255755483403,0.146036084380937,-0.946435303136844));
#4567=CARTESIAN_POINT('Ctrl Pts',(1.36511359324264,0.167235369334923,-1.06646836094372));
#4568=CARTESIAN_POINT('Ctrl Pts',(1.18480286160083,0.216895387258446,-1.33771622745885));
#4569=CARTESIAN_POINT('Ctrl Pts',(1.03366605550938,0.247409205792169,-1.5081345966626));
#4570=CARTESIAN_POINT('Ctrl Pts',(0.585735228688806,0.319098797267994,-1.8037064814823));
#4571=CARTESIAN_POINT('Ctrl Pts',(0.344445827034462,0.355553556198311,-1.90155408525721));
#4572=CARTESIAN_POINT('Ctrl Pts',(0.0608150575562096,0.395936422252363,
-1.95522821977963));
#4573=CARTESIAN_POINT('Ctrl Pts',(0.030455422336093,0.400230280246623,-1.96023027994078));
#4574=CARTESIAN_POINT('Ctrl Pts',(1.97280240755613E-8,0.404509616171237,
-1.96450961617124));
#4575=CARTESIAN_POINT('Origin',(0.,9.65431457505077,0.));
#4576=CARTESIAN_POINT('',(-2.59276989545945E-16,9.93715728752539,-2.11715728752538));
#4577=CARTESIAN_POINT('Origin',(0.,9.93715728752539,0.));
#4578=CARTESIAN_POINT('Origin',(-2.93915231795365E-16,9.65431457505077,
-2.4));
#4579=CARTESIAN_POINT('Origin',(0.,11.9,0.));
#4580=CARTESIAN_POINT('',(-4.82336772927411E-16,12.,-3.9385786437627));
#4581=CARTESIAN_POINT('Origin',(0.,12.,0.));
#4582=CARTESIAN_POINT('',(-4.90996333489766E-16,11.8292893218814,-4.00928932188135));
#4583=CARTESIAN_POINT('Origin',(-4.82336772927411E-16,11.9,-3.9385786437627));
#4584=CARTESIAN_POINT('Origin',(0.,11.8292893218814,0.));
#4585=CARTESIAN_POINT('Origin',(0.,9.82000000000001,0.));
#4586=CARTESIAN_POINT('',(-2.44929359829471E-16,9.82000000000001,-2.));
#4587=CARTESIAN_POINT('Origin',(0.,0.45,0.));
#4588=CARTESIAN_POINT('',(-0.257142857142752,0.440000000000001,-1.983400501921));
#4589=CARTESIAN_POINT('Ctrl Pts',(1.97280240755613E-8,0.404509616171237,
-1.96450961617124));
#4590=CARTESIAN_POINT('Ctrl Pts',(-0.0851508098666215,0.416474291496151,
-1.97647429235125));
#4591=CARTESIAN_POINT('Ctrl Pts',(-0.171050352799175,0.428324849718101,
-1.98278931537122));
#4592=CARTESIAN_POINT('Ctrl Pts',(-0.257142860795768,0.440000000495393,
-1.98340050194693));
#4593=CARTESIAN_POINT('Origin',(0.,0.440000000000001,0.));
#4594=CARTESIAN_POINT('Origin',(0.,70.,0.));
#4595=CARTESIAN_POINT('',(3.88911999139645E-5,0.512497733258513,-1.99999999962187));
#4596=CARTESIAN_POINT('Ctrl Pts',(7.41933818794109E-16,0.862500001911838,
2.));
#4597=CARTESIAN_POINT('Ctrl Pts',(-0.0552703432441355,0.85927589855593,
2.));
#4598=CARTESIAN_POINT('Ctrl Pts',(-0.110605204112353,0.856048031671933,
1.99770894428596));
#4599=CARTESIAN_POINT('Ctrl Pts',(-0.420525197530566,0.837969365389204,
1.97191801653875));
#4600=CARTESIAN_POINT('Ctrl Pts',(-0.668822497164996,0.823485356243864,
1.90210933332907));
#4601=CARTESIAN_POINT('Ctrl Pts',(-1.13407308457661,0.796345738644854,1.66855652158443));
#4602=CARTESIAN_POINT('Ctrl Pts',(-1.34493079919103,0.782575416162501,1.50380074095044));
#4603=CARTESIAN_POINT('Ctrl Pts',(-1.68839639792481,0.75234409837338,1.10367580094517));
#4604=CARTESIAN_POINT('Ctrl Pts',(-1.81842083590996,0.736898436276265,0.873000627974349));
#4605=CARTESIAN_POINT('Ctrl Pts',(-1.97923207905364,0.707461727060999,0.38314931713809));
#4606=CARTESIAN_POINT('Ctrl Pts',(-2.01178745902749,0.694397241615903,0.129724445636981));
#4607=CARTESIAN_POINT('Ctrl Pts',(-1.97990252339381,0.667327612876277,-0.38770646183827));
#4608=CARTESIAN_POINT('Ctrl Pts',(-1.91110912213568,0.652247930485477,-0.646488870964808));
#4609=CARTESIAN_POINT('Ctrl Pts',(-1.67927651187011,0.62172721310498,-1.11679377315213));
#4610=CARTESIAN_POINT('Ctrl Pts',(-1.52053416600623,0.606587237749995,-1.32483762606637));
#4611=CARTESIAN_POINT('Ctrl Pts',(-1.14842110785954,0.579074246128193,-1.65461404442982));
#4612=CARTESIAN_POINT('Ctrl Pts',(-0.943653674653732,0.567546466266641,
-1.77936282934091));
#4613=CARTESIAN_POINT('Ctrl Pts',(-0.491508565968716,0.541171334926682,
-1.95432023904762));
#4614=CARTESIAN_POINT('Ctrl Pts',(-0.246785668814814,0.526895832592705,
-2.00000479927351));
#4615=CARTESIAN_POINT('Ctrl Pts',(3.88911998226715E-5,0.512497733258518,
-1.99999999962187));
#4616=CARTESIAN_POINT('Ctrl Pts',(3.88911998825542E-5,0.512497733258514,
-1.99999999962187));
#4617=CARTESIAN_POINT('Ctrl Pts',(0.172907047386434,0.502413757480966,-1.99999663809686));
#4618=CARTESIAN_POINT('Ctrl Pts',(0.345047132249512,0.492372252530618,-1.97758246327963));
#4619=CARTESIAN_POINT('Ctrl Pts',(0.710657412499713,0.471044986182691,-1.88072556043873));
#4620=CARTESIAN_POINT('Ctrl Pts',(0.899787219881527,0.460416896217352,-1.79791535289817));
#4621=CARTESIAN_POINT('Ctrl Pts',(1.07297685035835,0.449803484035599,-1.68781535678376));
#4622=CARTESIAN_POINT('Ctrl Pts',(-0.257142857142745,0.440000000000001,
-1.983400501921));
#4623=CARTESIAN_POINT('Ctrl Pts',(-0.481635713382096,0.453095416613961,
-1.95429557106834));
#4624=CARTESIAN_POINT('Ctrl Pts',(-0.699591640436684,0.465809512358811,
-1.88728564808705));
#4625=CARTESIAN_POINT('Ctrl Pts',(-1.1001273672762,0.489174096424447,-1.68497256298937));
#4626=CARTESIAN_POINT('Ctrl Pts',(-1.28046697101911,0.500590709856682,-1.55237102657148));
#4627=CARTESIAN_POINT('Ctrl Pts',(-1.61723343414184,0.527945616611,-1.20531651088329));
#4628=CARTESIAN_POINT('Ctrl Pts',(-1.76065753494044,0.543307978847312,-0.984026546458247));
#4629=CARTESIAN_POINT('Ctrl Pts',(-1.95580405938054,0.573697470973118,-0.495138509125262));
#4630=CARTESIAN_POINT('Ctrl Pts',(-2.00411916259232,0.588168923320128,-0.231816382286525));
#4631=CARTESIAN_POINT('Ctrl Pts',(-1.99550412590271,0.614665037838943,0.287696770244476));
#4632=CARTESIAN_POINT('Ctrl Pts',(-1.94272556814002,0.62890241602013,0.539052054300045));
#4633=CARTESIAN_POINT('Ctrl Pts',(-1.7419954325077,0.658928568404834,1.01752413058528));
#4634=CARTESIAN_POINT('Ctrl Pts',(-1.59237071225919,0.674463850180423,1.23865708487486));
#4635=CARTESIAN_POINT('Ctrl Pts',(-1.21961396478033,0.703899598653046,1.60612258395746));
#4636=CARTESIAN_POINT('Ctrl Pts',(-1.00163913819066,0.716571050272238,1.75037007568662));
#4637=CARTESIAN_POINT('Ctrl Pts',(-0.52412048953386,0.744426304777219,1.94720477377504));
#4638=CARTESIAN_POINT('Ctrl Pts',(-0.269351609796664,0.75928782276189,1.99843116295333));
#4639=CARTESIAN_POINT('Ctrl Pts',(-0.0079409294476568,0.774536779115582,
1.99998817825517));
#4640=CARTESIAN_POINT('Ctrl Pts',(-0.00397018014396892,0.774768406158276,
2.));
#4641=CARTESIAN_POINT('Ctrl Pts',(7.0652298666267E-16,0.775000000000008,
2.));
#4642=CARTESIAN_POINT('Ctrl Pts',(-1.6211138875,71.7812500009559,0.));
#4643=CARTESIAN_POINT('Ctrl Pts',(-1.6211138875,71.7229166676226,-0.935950539335166));
#4644=CARTESIAN_POINT('Ctrl Pts',(-0.81055694375,71.6645833342892,-1.40392580900275));
#4645=CARTESIAN_POINT('Ctrl Pts',(-1.14620883215705E-16,71.6062500009559,
-1.87190107867033));
#4646=CARTESIAN_POINT('Ctrl Pts',(0.81055694375,71.5479166676226,-1.40392580900275));
#4647=CARTESIAN_POINT('Ctrl Pts',(1.6211138875,71.4895833342893,-0.935950539335166));
#4648=CARTESIAN_POINT('Ctrl Pts',(1.6211138875,71.4312500009559,-1.9852919333802E-16));
#4649=CARTESIAN_POINT('Ctrl Pts',(1.6211138875,71.3729166676226,0.935950539335165));
#4650=CARTESIAN_POINT('Ctrl Pts',(0.810556943750001,71.3145833342893,1.40392580900275));
#4651=CARTESIAN_POINT('Ctrl Pts',(3.43862649647115E-16,71.2562500009559,
1.87190107867033));
#4652=CARTESIAN_POINT('Ctrl Pts',(-0.810556943749999,71.1979166676226,1.40392580900275));
#4653=CARTESIAN_POINT('Ctrl Pts',(-1.6211138875,71.1395833342893,0.935950539335167));
#4654=CARTESIAN_POINT('Ctrl Pts',(-1.6211138875,71.0812500009559,0.));
#4655=CARTESIAN_POINT('Ctrl Pts',(-1.6211138875,71.0229166676226,-0.935950539335166));
#4656=CARTESIAN_POINT('Ctrl Pts',(-0.81055694375,70.9645833342893,-1.40392580900275));
#4657=CARTESIAN_POINT('Ctrl Pts',(-1.14620883215705E-16,70.9062500009559,
-1.87190107867033));
#4658=CARTESIAN_POINT('Ctrl Pts',(0.81055694375,70.8479166676226,-1.40392580900275));
#4659=CARTESIAN_POINT('Ctrl Pts',(1.6211138875,70.7895833342893,-0.935950539335166));
#4660=CARTESIAN_POINT('Ctrl Pts',(1.6211138875,70.7312500009559,-1.9852919333802E-16));
#4661=CARTESIAN_POINT('Ctrl Pts',(1.6211138875,70.6729166676226,0.935950539335165));
#4662=CARTESIAN_POINT('Ctrl Pts',(0.810556943750001,70.6145833342893,1.40392580900275));
#4663=CARTESIAN_POINT('Ctrl Pts',(3.43862649647115E-16,70.5562500009559,
1.87190107867033));
#4664=CARTESIAN_POINT('Ctrl Pts',(-0.810556943749999,70.4979166676226,1.40392580900275));
#4665=CARTESIAN_POINT('Ctrl Pts',(-1.6211138875,70.4395833342893,0.935950539335167));
#4666=CARTESIAN_POINT('Ctrl Pts',(-1.6211138875,70.3812500009559,0.));
#4667=CARTESIAN_POINT('Ctrl Pts',(-1.6211138875,70.3229166676226,-0.935950539335166));
#4668=CARTESIAN_POINT('Ctrl Pts',(-0.81055694375,70.2645833342893,-1.40392580900275));
#4669=CARTESIAN_POINT('Ctrl Pts',(-1.14620883215705E-16,70.2062500009559,
-1.87190107867033));
#4670=CARTESIAN_POINT('Ctrl Pts',(0.81055694375,70.1479166676226,-1.40392580900275));
#4671=CARTESIAN_POINT('Ctrl Pts',(1.6211138875,70.0895833342893,-0.935950539335166));
#4672=CARTESIAN_POINT('Ctrl Pts',(1.6211138875,70.0312500009559,-1.9852919333802E-16));
#4673=CARTESIAN_POINT('Ctrl Pts',(1.6211138875,69.9729166676226,0.935950539335165));
#4674=CARTESIAN_POINT('Ctrl Pts',(0.810556943750001,69.9145833342892,1.40392580900275));
#4675=CARTESIAN_POINT('Ctrl Pts',(3.43862649647115E-16,69.8562500009559,
1.87190107867033));
#4676=CARTESIAN_POINT('Ctrl Pts',(-0.810556943749999,69.7979166676226,1.40392580900275));
#4677=CARTESIAN_POINT('Ctrl Pts',(-1.6211138875,69.7395833342893,0.935950539335167));
#4678=CARTESIAN_POINT('Ctrl Pts',(-1.6211138875,69.6812500009559,0.));
#4679=CARTESIAN_POINT('Ctrl Pts',(-1.6211138875,69.6229166676226,-0.935950539335166));
#4680=CARTESIAN_POINT('Ctrl Pts',(-0.81055694375,69.5645833342893,-1.40392580900275));
#4681=CARTESIAN_POINT('Ctrl Pts',(-1.14620883215705E-16,69.5062500009559,
-1.87190107867033));
#4682=CARTESIAN_POINT('Ctrl Pts',(0.81055694375,69.4479166676226,-1.40392580900275));
#4683=CARTESIAN_POINT('Ctrl Pts',(1.6211138875,69.3895833342893,-0.935950539335166));
#4684=CARTESIAN_POINT('Ctrl Pts',(1.6211138875,69.3312500009559,-1.9852919333802E-16));
#4685=CARTESIAN_POINT('Ctrl Pts',(1.6211138875,69.2729166676226,0.935950539335165));
#4686=CARTESIAN_POINT('Ctrl Pts',(0.810556943750001,69.2145833342893,1.40392580900275));
#4687=CARTESIAN_POINT('Ctrl Pts',(3.43862649647115E-16,69.1562500009559,
1.87190107867033));
#4688=CARTESIAN_POINT('Ctrl Pts',(-0.810556943749999,69.0979166676226,1.40392580900275));
#4689=CARTESIAN_POINT('Ctrl Pts',(-1.6211138875,69.0395833342892,0.935950539335167));
#4690=CARTESIAN_POINT('Ctrl Pts',(-1.6211138875,68.9812500009559,0.));
#4691=CARTESIAN_POINT('Ctrl Pts',(-1.6211138875,68.9229166676226,-0.935950539335166));
#4692=CARTESIAN_POINT('Ctrl Pts',(-0.81055694375,68.8645833342893,-1.40392580900275));
#4693=CARTESIAN_POINT('Ctrl Pts',(-1.14620883215705E-16,68.8062500009559,
-1.87190107867033));
#4694=CARTESIAN_POINT('Ctrl Pts',(0.81055694375,68.7479166676226,-1.40392580900275));
#4695=CARTESIAN_POINT('Ctrl Pts',(1.6211138875,68.6895833342893,-0.935950539335166));
#4696=CARTESIAN_POINT('Ctrl Pts',(1.6211138875,68.6312500009559,-1.9852919333802E-16));
#4697=CARTESIAN_POINT('Ctrl Pts',(1.6211138875,68.5729166676226,0.935950539335165));
#4698=CARTESIAN_POINT('Ctrl Pts',(0.810556943750001,68.5145833342893,1.40392580900275));
#4699=CARTESIAN_POINT('Ctrl Pts',(3.43862649647115E-16,68.4562500009559,
1.87190107867033));
#4700=CARTESIAN_POINT('Ctrl Pts',(-0.810556943749999,68.3979166676226,1.40392580900275));
#4701=CARTESIAN_POINT('Ctrl Pts',(-1.6211138875,68.3395833342893,0.935950539335167));
#4702=CARTESIAN_POINT('Ctrl Pts',(-1.6211138875,68.2812500009559,0.));
#4703=CARTESIAN_POINT('Ctrl Pts',(-1.6211138875,68.2229166676226,-0.935950539335166));
#4704=CARTESIAN_POINT('Ctrl Pts',(-0.81055694375,68.1645833342892,-1.40392580900275));
#4705=CARTESIAN_POINT('Ctrl Pts',(-1.14620883215705E-16,68.1062500009559,
-1.87190107867033));
#4706=CARTESIAN_POINT('Ctrl Pts',(0.81055694375,68.0479166676226,-1.40392580900275));
#4707=CARTESIAN_POINT('Ctrl Pts',(1.6211138875,67.9895833342893,-0.935950539335166));
#4708=CARTESIAN_POINT('Ctrl Pts',(1.6211138875,67.9312500009559,-1.9852919333802E-16));
#4709=CARTESIAN_POINT('Ctrl Pts',(1.6211138875,67.8729166676226,0.935950539335165));
#4710=CARTESIAN_POINT('Ctrl Pts',(0.810556943750001,67.8145833342893,1.40392580900275));
#4711=CARTESIAN_POINT('Ctrl Pts',(3.43862649647115E-16,67.7562500009559,
1.87190107867033));
#4712=CARTESIAN_POINT('Ctrl Pts',(-0.810556943749999,67.6979166676226,1.40392580900275));
#4713=CARTESIAN_POINT('Ctrl Pts',(-1.6211138875,67.6395833342893,0.935950539335167));
#4714=CARTESIAN_POINT('Ctrl Pts',(-1.6211138875,67.5812500009559,0.));
#4715=CARTESIAN_POINT('Ctrl Pts',(-1.6211138875,67.5229166676226,-0.935950539335166));
#4716=CARTESIAN_POINT('Ctrl Pts',(-0.81055694375,67.4645833342893,-1.40392580900275));
#4717=CARTESIAN_POINT('Ctrl Pts',(-1.14620883215705E-16,67.4062500009559,
-1.87190107867033));
#4718=CARTESIAN_POINT('Ctrl Pts',(0.81055694375,67.3479166676226,-1.40392580900275));
#4719=CARTESIAN_POINT('Ctrl Pts',(1.6211138875,67.2895833342892,-0.935950539335166));
#4720=CARTESIAN_POINT('Ctrl Pts',(1.6211138875,67.2312500009559,-1.9852919333802E-16));
#4721=CARTESIAN_POINT('Ctrl Pts',(1.6211138875,67.1729166676226,0.935950539335165));
#4722=CARTESIAN_POINT('Ctrl Pts',(0.810556943750001,67.1145833342893,1.40392580900275));
#4723=CARTESIAN_POINT('Ctrl Pts',(3.43862649647115E-16,67.0562500009559,
1.87190107867033));
#4724=CARTESIAN_POINT('Ctrl Pts',(-0.810556943749999,66.9979166676226,1.40392580900275));
#4725=CARTESIAN_POINT('Ctrl Pts',(-1.6211138875,66.9395833342893,0.935950539335167));
#4726=CARTESIAN_POINT('Ctrl Pts',(-1.6211138875,66.8812500009559,0.));
#4727=CARTESIAN_POINT('Ctrl Pts',(-1.6211138875,66.8229166676226,-0.935950539335166));
#4728=CARTESIAN_POINT('Ctrl Pts',(-0.81055694375,66.7645833342893,-1.40392580900275));
#4729=CARTESIAN_POINT('Ctrl Pts',(-1.14620883215705E-16,66.7062500009559,
-1.87190107867033));
#4730=CARTESIAN_POINT('Ctrl Pts',(0.81055694375,66.6479166676226,-1.40392580900275));
#4731=CARTESIAN_POINT('Ctrl Pts',(1.6211138875,66.5895833342893,-0.935950539335166));
#4732=CARTESIAN_POINT('Ctrl Pts',(1.6211138875,66.5312500009559,-1.9852919333802E-16));
#4733=CARTESIAN_POINT('Ctrl Pts',(1.6211138875,66.4729166676226,0.935950539335165));
#4734=CARTESIAN_POINT('Ctrl Pts',(0.810556943750001,66.4145833342893,1.40392580900275));
#4735=CARTESIAN_POINT('Ctrl Pts',(3.43862649647115E-16,66.3562500009559,
1.87190107867033));
#4736=CARTESIAN_POINT('Ctrl Pts',(-0.810556943749999,66.2979166676226,1.40392580900275));
#4737=CARTESIAN_POINT('Ctrl Pts',(-1.6211138875,66.2395833342893,0.935950539335167));
#4738=CARTESIAN_POINT('Ctrl Pts',(-1.6211138875,66.1812500009559,0.));
#4739=CARTESIAN_POINT('Ctrl Pts',(-1.6211138875,66.1229166676226,-0.935950539335166));
#4740=CARTESIAN_POINT('Ctrl Pts',(-0.81055694375,66.0645833342893,-1.40392580900275));
#4741=CARTESIAN_POINT('Ctrl Pts',(-1.14620883215705E-16,66.0062500009559,
-1.87190107867033));
#4742=CARTESIAN_POINT('Ctrl Pts',(0.81055694375,65.9479166676226,-1.40392580900275));
#4743=CARTESIAN_POINT('Ctrl Pts',(1.6211138875,65.8895833342893,-0.935950539335166));
#4744=CARTESIAN_POINT('Ctrl Pts',(1.6211138875,65.8312500009559,-1.9852919333802E-16));
#4745=CARTESIAN_POINT('Ctrl Pts',(1.6211138875,65.7729166676226,0.935950539335165));
#4746=CARTESIAN_POINT('Ctrl Pts',(0.810556943750001,65.7145833342893,1.40392580900275));
#4747=CARTESIAN_POINT('Ctrl Pts',(3.43862649647115E-16,65.6562500009559,
1.87190107867033));
#4748=CARTESIAN_POINT('Ctrl Pts',(-0.810556943749999,65.5979166676226,1.40392580900275));
#4749=CARTESIAN_POINT('Ctrl Pts',(-1.6211138875,65.5395833342892,0.935950539335167));
#4750=CARTESIAN_POINT('Ctrl Pts',(-1.6211138875,65.4812500009559,0.));
#4751=CARTESIAN_POINT('Ctrl Pts',(-1.6211138875,65.4229166676226,-0.935950539335166));
#4752=CARTESIAN_POINT('Ctrl Pts',(-0.81055694375,65.3645833342893,-1.40392580900275));
#4753=CARTESIAN_POINT('Ctrl Pts',(-1.14620883215705E-16,65.3062500009559,
-1.87190107867033));
#4754=CARTESIAN_POINT('Ctrl Pts',(0.81055694375,65.2479166676226,-1.40392580900275));
#4755=CARTESIAN_POINT('Ctrl Pts',(1.6211138875,65.1895833342893,-0.935950539335166));
#4756=CARTESIAN_POINT('Ctrl Pts',(1.6211138875,65.1312500009559,-1.9852919333802E-16));
#4757=CARTESIAN_POINT('Ctrl Pts',(1.6211138875,65.0729166676226,0.935950539335165));
#4758=CARTESIAN_POINT('Ctrl Pts',(0.810556943750001,65.0145833342893,1.40392580900275));
#4759=CARTESIAN_POINT('Ctrl Pts',(3.43862649647115E-16,64.9562500009559,
1.87190107867033));
#4760=CARTESIAN_POINT('Ctrl Pts',(-0.810556943749999,64.8979166676226,1.40392580900275));
#4761=CARTESIAN_POINT('Ctrl Pts',(-1.6211138875,64.8395833342893,0.935950539335167));
#4762=CARTESIAN_POINT('Ctrl Pts',(-1.6211138875,64.7812500009559,0.));
#4763=CARTESIAN_POINT('Ctrl Pts',(-1.6211138875,64.7229166676226,-0.935950539335166));
#4764=CARTESIAN_POINT('Ctrl Pts',(-0.81055694375,64.6645833342893,-1.40392580900275));
#4765=CARTESIAN_POINT('Ctrl Pts',(-1.14620883215705E-16,64.6062500009559,
-1.87190107867033));
#4766=CARTESIAN_POINT('Ctrl Pts',(0.81055694375,64.5479166676226,-1.40392580900275));
#4767=CARTESIAN_POINT('Ctrl Pts',(1.6211138875,64.4895833342893,-0.935950539335166));
#4768=CARTESIAN_POINT('Ctrl Pts',(1.6211138875,64.4312500009559,-1.9852919333802E-16));
#4769=CARTESIAN_POINT('Ctrl Pts',(1.6211138875,64.3729166676226,0.935950539335165));
#4770=CARTESIAN_POINT('Ctrl Pts',(0.810556943750001,64.3145833342893,1.40392580900275));
#4771=CARTESIAN_POINT('Ctrl Pts',(3.43862649647115E-16,64.2562500009559,
1.87190107867033));
#4772=CARTESIAN_POINT('Ctrl Pts',(-0.810556943749999,64.1979166676226,1.40392580900275));
#4773=CARTESIAN_POINT('Ctrl Pts',(-1.6211138875,64.1395833342893,0.935950539335167));
#4774=CARTESIAN_POINT('Ctrl Pts',(-1.6211138875,64.0812500009559,0.));
#4775=CARTESIAN_POINT('Ctrl Pts',(-1.6211138875,64.0229166676226,-0.935950539335166));
#4776=CARTESIAN_POINT('Ctrl Pts',(-0.81055694375,63.9645833342893,-1.40392580900275));
#4777=CARTESIAN_POINT('Ctrl Pts',(-1.14620883215705E-16,63.9062500009559,
-1.87190107867033));
#4778=CARTESIAN_POINT('Ctrl Pts',(0.81055694375,63.8479166676226,-1.40392580900275));
#4779=CARTESIAN_POINT('Ctrl Pts',(1.6211138875,63.7895833342893,-0.935950539335166));
#4780=CARTESIAN_POINT('Ctrl Pts',(1.6211138875,63.7312500009559,-1.9852919333802E-16));
#4781=CARTESIAN_POINT('Ctrl Pts',(1.6211138875,63.6729166676226,0.935950539335165));
#4782=CARTESIAN_POINT('Ctrl Pts',(0.810556943750001,63.6145833342893,1.40392580900275));
#4783=CARTESIAN_POINT('Ctrl Pts',(3.43862649647115E-16,63.5562500009559,
1.87190107867033));
#4784=CARTESIAN_POINT('Ctrl Pts',(-0.810556943749999,63.4979166676226,1.40392580900275));
#4785=CARTESIAN_POINT('Ctrl Pts',(-1.6211138875,63.4395833342893,0.935950539335167));
#4786=CARTESIAN_POINT('Ctrl Pts',(-1.6211138875,63.3812500009559,0.));
#4787=CARTESIAN_POINT('Ctrl Pts',(-1.6211138875,63.3229166676226,-0.935950539335166));
#4788=CARTESIAN_POINT('Ctrl Pts',(-0.81055694375,63.2645833342892,-1.40392580900275));
#4789=CARTESIAN_POINT('Ctrl Pts',(-1.14620883215705E-16,63.2062500009559,
-1.87190107867033));
#4790=CARTESIAN_POINT('Ctrl Pts',(0.81055694375,63.1479166676226,-1.40392580900275));
#4791=CARTESIAN_POINT('Ctrl Pts',(1.6211138875,63.0895833342893,-0.935950539335166));
#4792=CARTESIAN_POINT('Ctrl Pts',(1.6211138875,63.0312500009559,-1.9852919333802E-16));
#4793=CARTESIAN_POINT('Ctrl Pts',(1.6211138875,62.9729166676226,0.935950539335165));
#4794=CARTESIAN_POINT('Ctrl Pts',(0.810556943750001,62.9145833342893,1.40392580900275));
#4795=CARTESIAN_POINT('Ctrl Pts',(3.43862649647115E-16,62.8562500009559,
1.87190107867033));
#4796=CARTESIAN_POINT('Ctrl Pts',(-0.810556943749999,62.7979166676226,1.40392580900275));
#4797=CARTESIAN_POINT('Ctrl Pts',(-1.6211138875,62.7395833342893,0.935950539335167));
#4798=CARTESIAN_POINT('Ctrl Pts',(-1.6211138875,62.6812500009559,0.));
#4799=CARTESIAN_POINT('Ctrl Pts',(-1.6211138875,62.6229166676226,-0.935950539335166));
#4800=CARTESIAN_POINT('Ctrl Pts',(-0.81055694375,62.5645833342893,-1.40392580900275));
#4801=CARTESIAN_POINT('Ctrl Pts',(-1.14620883215705E-16,62.5062500009559,
-1.87190107867033));
#4802=CARTESIAN_POINT('Ctrl Pts',(0.81055694375,62.4479166676226,-1.40392580900275));
#4803=CARTESIAN_POINT('Ctrl Pts',(1.6211138875,62.3895833342893,-0.935950539335166));
#4804=CARTESIAN_POINT('Ctrl Pts',(1.6211138875,62.3312500009559,-1.9852919333802E-16));
#4805=CARTESIAN_POINT('Ctrl Pts',(1.6211138875,62.2729166676226,0.935950539335165));
#4806=CARTESIAN_POINT('Ctrl Pts',(0.810556943750001,62.2145833342893,1.40392580900275));
#4807=CARTESIAN_POINT('Ctrl Pts',(3.43862649647115E-16,62.1562500009559,
1.87190107867033));
#4808=CARTESIAN_POINT('Ctrl Pts',(-0.810556943749999,62.0979166676226,1.40392580900275));
#4809=CARTESIAN_POINT('Ctrl Pts',(-1.6211138875,62.0395833342893,0.935950539335167));
#4810=CARTESIAN_POINT('Ctrl Pts',(-1.6211138875,61.9812500009559,0.));
#4811=CARTESIAN_POINT('Ctrl Pts',(-1.6211138875,61.9229166676226,-0.935950539335166));
#4812=CARTESIAN_POINT('Ctrl Pts',(-0.81055694375,61.8645833342893,-1.40392580900275));
#4813=CARTESIAN_POINT('Ctrl Pts',(-1.14620883215705E-16,61.8062500009559,
-1.87190107867033));
#4814=CARTESIAN_POINT('Ctrl Pts',(0.81055694375,61.7479166676226,-1.40392580900275));
#4815=CARTESIAN_POINT('Ctrl Pts',(1.6211138875,61.6895833342893,-0.935950539335166));
#4816=CARTESIAN_POINT('Ctrl Pts',(1.6211138875,61.6312500009559,-1.9852919333802E-16));
#4817=CARTESIAN_POINT('Ctrl Pts',(1.6211138875,61.5729166676226,0.935950539335165));
#4818=CARTESIAN_POINT('Ctrl Pts',(0.810556943750001,61.5145833342893,1.40392580900275));
#4819=CARTESIAN_POINT('Ctrl Pts',(3.43862649647115E-16,61.4562500009559,
1.87190107867033));
#4820=CARTESIAN_POINT('Ctrl Pts',(-0.810556943749999,61.3979166676226,1.40392580900275));
#4821=CARTESIAN_POINT('Ctrl Pts',(-1.6211138875,61.3395833342893,0.935950539335167));
#4822=CARTESIAN_POINT('Ctrl Pts',(-1.6211138875,61.2812500009559,0.));
#4823=CARTESIAN_POINT('Ctrl Pts',(-1.6211138875,61.2229166676226,-0.935950539335166));
#4824=CARTESIAN_POINT('Ctrl Pts',(-0.81055694375,61.1645833342893,-1.40392580900275));
#4825=CARTESIAN_POINT('Ctrl Pts',(-1.14620883215705E-16,61.1062500009559,
-1.87190107867033));
#4826=CARTESIAN_POINT('Ctrl Pts',(0.81055694375,61.0479166676226,-1.40392580900275));
#4827=CARTESIAN_POINT('Ctrl Pts',(1.6211138875,60.9895833342893,-0.935950539335166));
#4828=CARTESIAN_POINT('Ctrl Pts',(1.6211138875,60.9312500009559,-1.9852919333802E-16));
#4829=CARTESIAN_POINT('Ctrl Pts',(1.6211138875,60.8729166676226,0.935950539335165));
#4830=CARTESIAN_POINT('Ctrl Pts',(0.810556943750001,60.8145833342893,1.40392580900275));
#4831=CARTESIAN_POINT('Ctrl Pts',(3.43862649647115E-16,60.7562500009559,
1.87190107867033));
#4832=CARTESIAN_POINT('Ctrl Pts',(-0.810556943749999,60.6979166676226,1.40392580900275));
#4833=CARTESIAN_POINT('Ctrl Pts',(-1.6211138875,60.6395833342892,0.935950539335167));
#4834=CARTESIAN_POINT('Ctrl Pts',(-1.6211138875,60.5812500009559,0.));
#4835=CARTESIAN_POINT('Ctrl Pts',(-1.6211138875,60.5229166676226,-0.935950539335166));
#4836=CARTESIAN_POINT('Ctrl Pts',(-0.81055694375,60.4645833342893,-1.40392580900275));
#4837=CARTESIAN_POINT('Ctrl Pts',(-1.14620883215705E-16,60.4062500009559,
-1.87190107867033));
#4838=CARTESIAN_POINT('Ctrl Pts',(0.81055694375,60.3479166676226,-1.40392580900275));
#4839=CARTESIAN_POINT('Ctrl Pts',(1.6211138875,60.2895833342893,-0.935950539335166));
#4840=CARTESIAN_POINT('Ctrl Pts',(1.6211138875,60.2312500009559,-1.9852919333802E-16));
#4841=CARTESIAN_POINT('Ctrl Pts',(1.6211138875,60.1729166676226,0.935950539335165));
#4842=CARTESIAN_POINT('Ctrl Pts',(0.810556943750001,60.1145833342893,1.40392580900275));
#4843=CARTESIAN_POINT('Ctrl Pts',(3.43862649647115E-16,60.0562500009559,
1.87190107867033));
#4844=CARTESIAN_POINT('Ctrl Pts',(-0.810556943749999,59.9979166676226,1.40392580900275));
#4845=CARTESIAN_POINT('Ctrl Pts',(-1.6211138875,59.9395833342893,0.935950539335167));
#4846=CARTESIAN_POINT('Ctrl Pts',(-1.6211138875,59.8812500009559,0.));
#4847=CARTESIAN_POINT('Ctrl Pts',(-1.6211138875,59.8229166676226,-0.935950539335166));
#4848=CARTESIAN_POINT('Ctrl Pts',(-0.81055694375,59.7645833342893,-1.40392580900275));
#4849=CARTESIAN_POINT('Ctrl Pts',(-1.14620883215705E-16,59.7062500009559,
-1.87190107867033));
#4850=CARTESIAN_POINT('Ctrl Pts',(0.81055694375,59.6479166676226,-1.40392580900275));
#4851=CARTESIAN_POINT('Ctrl Pts',(1.6211138875,59.5895833342893,-0.935950539335166));
#4852=CARTESIAN_POINT('Ctrl Pts',(1.6211138875,59.5312500009559,-1.9852919333802E-16));
#4853=CARTESIAN_POINT('Ctrl Pts',(1.6211138875,59.4729166676226,0.935950539335165));
#4854=CARTESIAN_POINT('Ctrl Pts',(0.810556943750001,59.4145833342893,1.40392580900275));
#4855=CARTESIAN_POINT('Ctrl Pts',(3.43862649647115E-16,59.3562500009559,
1.87190107867033));
#4856=CARTESIAN_POINT('Ctrl Pts',(-0.810556943749999,59.2979166676226,1.40392580900275));
#4857=CARTESIAN_POINT('Ctrl Pts',(-1.6211138875,59.2395833342893,0.935950539335167));
#4858=CARTESIAN_POINT('Ctrl Pts',(-1.6211138875,59.1812500009559,0.));
#4859=CARTESIAN_POINT('Ctrl Pts',(-1.6211138875,59.1229166676226,-0.935950539335166));
#4860=CARTESIAN_POINT('Ctrl Pts',(-0.81055694375,59.0645833342893,-1.40392580900275));
#4861=CARTESIAN_POINT('Ctrl Pts',(-1.14620883215705E-16,59.0062500009559,
-1.87190107867033));
#4862=CARTESIAN_POINT('Ctrl Pts',(0.81055694375,58.9479166676226,-1.40392580900275));
#4863=CARTESIAN_POINT('Ctrl Pts',(1.6211138875,58.8895833342893,-0.935950539335166));
#4864=CARTESIAN_POINT('Ctrl Pts',(1.6211138875,58.8312500009559,-1.9852919333802E-16));
#4865=CARTESIAN_POINT('Ctrl Pts',(1.6211138875,58.7729166676226,0.935950539335165));
#4866=CARTESIAN_POINT('Ctrl Pts',(0.810556943750001,58.7145833342893,1.40392580900275));
#4867=CARTESIAN_POINT('Ctrl Pts',(3.43862649647115E-16,58.6562500009559,
1.87190107867033));
#4868=CARTESIAN_POINT('Ctrl Pts',(-0.810556943749999,58.5979166676226,1.40392580900275));
#4869=CARTESIAN_POINT('Ctrl Pts',(-1.6211138875,58.5395833342892,0.935950539335167));
#4870=CARTESIAN_POINT('Ctrl Pts',(-1.6211138875,58.4812500009559,0.));
#4871=CARTESIAN_POINT('Ctrl Pts',(-1.6211138875,58.4229166676226,-0.935950539335166));
#4872=CARTESIAN_POINT('Ctrl Pts',(-0.81055694375,58.3645833342893,-1.40392580900275));
#4873=CARTESIAN_POINT('Ctrl Pts',(-1.14620883215705E-16,58.3062500009559,
-1.87190107867033));
#4874=CARTESIAN_POINT('Ctrl Pts',(0.81055694375,58.2479166676226,-1.40392580900275));
#4875=CARTESIAN_POINT('Ctrl Pts',(1.6211138875,58.1895833342893,-0.935950539335166));
#4876=CARTESIAN_POINT('Ctrl Pts',(1.6211138875,58.1312500009559,-1.9852919333802E-16));
#4877=CARTESIAN_POINT('Ctrl Pts',(1.6211138875,58.0729166676226,0.935950539335165));
#4878=CARTESIAN_POINT('Ctrl Pts',(0.810556943750001,58.0145833342893,1.40392580900275));
#4879=CARTESIAN_POINT('Ctrl Pts',(3.43862649647115E-16,57.9562500009559,
1.87190107867033));
#4880=CARTESIAN_POINT('Ctrl Pts',(-0.810556943749999,57.8979166676226,1.40392580900275));
#4881=CARTESIAN_POINT('Ctrl Pts',(-1.6211138875,57.8395833342893,0.935950539335167));
#4882=CARTESIAN_POINT('Ctrl Pts',(-1.6211138875,57.7812500009559,0.));
#4883=CARTESIAN_POINT('Ctrl Pts',(-1.6211138875,57.7229166676226,-0.935950539335166));
#4884=CARTESIAN_POINT('Ctrl Pts',(-0.81055694375,57.6645833342893,-1.40392580900275));
#4885=CARTESIAN_POINT('Ctrl Pts',(-1.14620883215705E-16,57.6062500009559,
-1.87190107867033));
#4886=CARTESIAN_POINT('Ctrl Pts',(0.81055694375,57.5479166676226,-1.40392580900275));
#4887=CARTESIAN_POINT('Ctrl Pts',(1.6211138875,57.4895833342893,-0.935950539335166));
#4888=CARTESIAN_POINT('Ctrl Pts',(1.6211138875,57.4312500009559,-1.9852919333802E-16));
#4889=CARTESIAN_POINT('Ctrl Pts',(1.6211138875,57.3729166676226,0.935950539335165));
#4890=CARTESIAN_POINT('Ctrl Pts',(0.810556943750001,57.3145833342893,1.40392580900275));
#4891=CARTESIAN_POINT('Ctrl Pts',(3.43862649647115E-16,57.2562500009559,
1.87190107867033));
#4892=CARTESIAN_POINT('Ctrl Pts',(-0.810556943749999,57.1979166676226,1.40392580900275));
#4893=CARTESIAN_POINT('Ctrl Pts',(-1.6211138875,57.1395833342893,0.935950539335167));
#4894=CARTESIAN_POINT('Ctrl Pts',(-1.6211138875,57.0812500009559,0.));
#4895=CARTESIAN_POINT('Ctrl Pts',(-1.6211138875,57.0229166676226,-0.935950539335166));
#4896=CARTESIAN_POINT('Ctrl Pts',(-0.81055694375,56.9645833342893,-1.40392580900275));
#4897=CARTESIAN_POINT('Ctrl Pts',(-1.14620883215705E-16,56.9062500009559,
-1.87190107867033));
#4898=CARTESIAN_POINT('Ctrl Pts',(0.81055694375,56.8479166676226,-1.40392580900275));
#4899=CARTESIAN_POINT('Ctrl Pts',(1.6211138875,56.7895833342892,-0.935950539335166));
#4900=CARTESIAN_POINT('Ctrl Pts',(1.6211138875,56.7312500009559,-1.9852919333802E-16));
#4901=CARTESIAN_POINT('Ctrl Pts',(1.6211138875,56.6729166676226,0.935950539335165));
#4902=CARTESIAN_POINT('Ctrl Pts',(0.810556943750001,56.6145833342893,1.40392580900275));
#4903=CARTESIAN_POINT('Ctrl Pts',(3.43862649647115E-16,56.5562500009559,
1.87190107867033));
#4904=CARTESIAN_POINT('Ctrl Pts',(-0.810556943749999,56.4979166676226,1.40392580900275));
#4905=CARTESIAN_POINT('Ctrl Pts',(-1.6211138875,56.4395833342893,0.935950539335167));
#4906=CARTESIAN_POINT('Ctrl Pts',(-1.6211138875,56.3812500009559,0.));
#4907=CARTESIAN_POINT('Ctrl Pts',(-1.6211138875,56.3229166676226,-0.935950539335166));
#4908=CARTESIAN_POINT('Ctrl Pts',(-0.81055694375,56.2645833342893,-1.40392580900275));
#4909=CARTESIAN_POINT('Ctrl Pts',(-1.14620883215705E-16,56.2062500009559,
-1.87190107867033));
#4910=CARTESIAN_POINT('Ctrl Pts',(0.81055694375,56.1479166676226,-1.40392580900275));
#4911=CARTESIAN_POINT('Ctrl Pts',(1.6211138875,56.0895833342893,-0.935950539335166));
#4912=CARTESIAN_POINT('Ctrl Pts',(1.6211138875,56.0312500009559,-1.9852919333802E-16));
#4913=CARTESIAN_POINT('Ctrl Pts',(1.6211138875,55.9729166676226,0.935950539335165));
#4914=CARTESIAN_POINT('Ctrl Pts',(0.810556943750001,55.9145833342893,1.40392580900275));
#4915=CARTESIAN_POINT('Ctrl Pts',(3.43862649647115E-16,55.8562500009559,
1.87190107867033));
#4916=CARTESIAN_POINT('Ctrl Pts',(-0.810556943749999,55.7979166676226,1.40392580900275));
#4917=CARTESIAN_POINT('Ctrl Pts',(-1.6211138875,55.7395833342893,0.935950539335167));
#4918=CARTESIAN_POINT('Ctrl Pts',(-1.6211138875,55.6812500009559,0.));
#4919=CARTESIAN_POINT('Ctrl Pts',(-1.6211138875,55.6229166676226,-0.935950539335166));
#4920=CARTESIAN_POINT('Ctrl Pts',(-0.81055694375,55.5645833342893,-1.40392580900275));
#4921=CARTESIAN_POINT('Ctrl Pts',(-1.14620883215705E-16,55.5062500009559,
-1.87190107867033));
#4922=CARTESIAN_POINT('Ctrl Pts',(0.81055694375,55.4479166676226,-1.40392580900275));
#4923=CARTESIAN_POINT('Ctrl Pts',(1.6211138875,55.3895833342893,-0.935950539335166));
#4924=CARTESIAN_POINT('Ctrl Pts',(1.6211138875,55.3312500009559,-1.9852919333802E-16));
#4925=CARTESIAN_POINT('Ctrl Pts',(1.6211138875,55.2729166676226,0.935950539335165));
#4926=CARTESIAN_POINT('Ctrl Pts',(0.810556943750001,55.2145833342893,1.40392580900275));
#4927=CARTESIAN_POINT('Ctrl Pts',(3.43862649647115E-16,55.1562500009559,
1.87190107867033));
#4928=CARTESIAN_POINT('Ctrl Pts',(-0.810556943749999,55.0979166676226,1.40392580900275));
#4929=CARTESIAN_POINT('Ctrl Pts',(-1.6211138875,55.0395833342893,0.935950539335167));
#4930=CARTESIAN_POINT('Ctrl Pts',(-1.6211138875,54.9812500009559,0.));
#4931=CARTESIAN_POINT('Ctrl Pts',(-1.6211138875,54.9229166676226,-0.935950539335166));
#4932=CARTESIAN_POINT('Ctrl Pts',(-0.81055694375,54.8645833342893,-1.40392580900275));
#4933=CARTESIAN_POINT('Ctrl Pts',(-1.14620883215705E-16,54.8062500009559,
-1.87190107867033));
#4934=CARTESIAN_POINT('Ctrl Pts',(0.81055694375,54.7479166676226,-1.40392580900275));
#4935=CARTESIAN_POINT('Ctrl Pts',(1.6211138875,54.6895833342893,-0.935950539335166));
#4936=CARTESIAN_POINT('Ctrl Pts',(1.6211138875,54.6312500009559,-1.9852919333802E-16));
#4937=CARTESIAN_POINT('Ctrl Pts',(1.6211138875,54.5729166676226,0.935950539335165));
#4938=CARTESIAN_POINT('Ctrl Pts',(0.810556943750001,54.5145833342893,1.40392580900275));
#4939=CARTESIAN_POINT('Ctrl Pts',(3.43862649647115E-16,54.4562500009559,
1.87190107867033));
#4940=CARTESIAN_POINT('Ctrl Pts',(-0.810556943749999,54.3979166676226,1.40392580900275));
#4941=CARTESIAN_POINT('Ctrl Pts',(-1.6211138875,54.3395833342893,0.935950539335167));
#4942=CARTESIAN_POINT('Ctrl Pts',(-1.6211138875,54.2812500009559,0.));
#4943=CARTESIAN_POINT('Ctrl Pts',(-1.6211138875,54.2229166676226,-0.935950539335166));
#4944=CARTESIAN_POINT('Ctrl Pts',(-0.81055694375,54.1645833342893,-1.40392580900275));
#4945=CARTESIAN_POINT('Ctrl Pts',(-1.14620883215705E-16,54.1062500009559,
-1.87190107867033));
#4946=CARTESIAN_POINT('Ctrl Pts',(0.81055694375,54.0479166676226,-1.40392580900275));
#4947=CARTESIAN_POINT('Ctrl Pts',(1.6211138875,53.9895833342893,-0.935950539335166));
#4948=CARTESIAN_POINT('Ctrl Pts',(1.6211138875,53.9312500009559,-1.9852919333802E-16));
#4949=CARTESIAN_POINT('Ctrl Pts',(1.6211138875,53.8729166676226,0.935950539335165));
#4950=CARTESIAN_POINT('Ctrl Pts',(0.810556943750001,53.8145833342893,1.40392580900275));
#4951=CARTESIAN_POINT('Ctrl Pts',(3.43862649647115E-16,53.7562500009559,
1.87190107867033));
#4952=CARTESIAN_POINT('Ctrl Pts',(-0.810556943749999,53.6979166676226,1.40392580900275));
#4953=CARTESIAN_POINT('Ctrl Pts',(-1.6211138875,53.6395833342893,0.935950539335167));
#4954=CARTESIAN_POINT('Ctrl Pts',(-1.6211138875,53.5812500009559,0.));
#4955=CARTESIAN_POINT('Ctrl Pts',(-1.6211138875,53.5229166676226,-0.935950539335166));
#4956=CARTESIAN_POINT('Ctrl Pts',(-0.81055694375,53.4645833342893,-1.40392580900275));
#4957=CARTESIAN_POINT('Ctrl Pts',(-1.14620883215705E-16,53.4062500009559,
-1.87190107867033));
#4958=CARTESIAN_POINT('Ctrl Pts',(0.81055694375,53.3479166676226,-1.40392580900275));
#4959=CARTESIAN_POINT('Ctrl Pts',(1.6211138875,53.2895833342893,-0.935950539335166));
#4960=CARTESIAN_POINT('Ctrl Pts',(1.6211138875,53.2312500009559,-1.9852919333802E-16));
#4961=CARTESIAN_POINT('Ctrl Pts',(1.6211138875,53.1729166676226,0.935950539335165));
#4962=CARTESIAN_POINT('Ctrl Pts',(0.810556943750001,53.1145833342893,1.40392580900275));
#4963=CARTESIAN_POINT('Ctrl Pts',(3.43862649647115E-16,53.0562500009559,
1.87190107867033));
#4964=CARTESIAN_POINT('Ctrl Pts',(-0.810556943749999,52.9979166676226,1.40392580900275));
#4965=CARTESIAN_POINT('Ctrl Pts',(-1.6211138875,52.9395833342893,0.935950539335167));
#4966=CARTESIAN_POINT('Ctrl Pts',(-1.6211138875,52.8812500009559,0.));
#4967=CARTESIAN_POINT('Ctrl Pts',(-1.6211138875,52.8229166676226,-0.935950539335166));
#4968=CARTESIAN_POINT('Ctrl Pts',(-0.81055694375,52.7645833342893,-1.40392580900275));
#4969=CARTESIAN_POINT('Ctrl Pts',(-1.14620883215705E-16,52.7062500009559,
-1.87190107867033));
#4970=CARTESIAN_POINT('Ctrl Pts',(0.81055694375,52.6479166676226,-1.40392580900275));
#4971=CARTESIAN_POINT('Ctrl Pts',(1.6211138875,52.5895833342892,-0.935950539335166));
#4972=CARTESIAN_POINT('Ctrl Pts',(1.6211138875,52.5312500009559,-1.9852919333802E-16));
#4973=CARTESIAN_POINT('Ctrl Pts',(1.6211138875,52.4729166676226,0.935950539335165));
#4974=CARTESIAN_POINT('Ctrl Pts',(0.810556943750001,52.4145833342892,1.40392580900275));
#4975=CARTESIAN_POINT('Ctrl Pts',(3.43862649647115E-16,52.3562500009559,
1.87190107867033));
#4976=CARTESIAN_POINT('Ctrl Pts',(-0.810556943749999,52.2979166676226,1.40392580900275));
#4977=CARTESIAN_POINT('Ctrl Pts',(-1.6211138875,52.2395833342893,0.935950539335167));
#4978=CARTESIAN_POINT('Ctrl Pts',(-1.6211138875,52.1812500009559,0.));
#4979=CARTESIAN_POINT('Ctrl Pts',(-1.6211138875,52.1229166676226,-0.935950539335166));
#4980=CARTESIAN_POINT('Ctrl Pts',(-0.81055694375,52.0645833342893,-1.40392580900275));
#4981=CARTESIAN_POINT('Ctrl Pts',(-1.14620883215705E-16,52.0062500009559,
-1.87190107867033));
#4982=CARTESIAN_POINT('Ctrl Pts',(0.81055694375,51.9479166676226,-1.40392580900275));
#4983=CARTESIAN_POINT('Ctrl Pts',(1.6211138875,51.8895833342892,-0.935950539335166));
#4984=CARTESIAN_POINT('Ctrl Pts',(1.6211138875,51.8312500009559,-1.9852919333802E-16));
#4985=CARTESIAN_POINT('Ctrl Pts',(1.6211138875,51.7729166676226,0.935950539335165));
#4986=CARTESIAN_POINT('Ctrl Pts',(0.810556943750001,51.7145833342893,1.40392580900275));
#4987=CARTESIAN_POINT('Ctrl Pts',(3.43862649647115E-16,51.6562500009559,
1.87190107867033));
#4988=CARTESIAN_POINT('Ctrl Pts',(-0.810556943749999,51.5979166676226,1.40392580900275));
#4989=CARTESIAN_POINT('Ctrl Pts',(-1.6211138875,51.5395833342893,0.935950539335167));
#4990=CARTESIAN_POINT('Ctrl Pts',(-1.6211138875,51.4812500009559,0.));
#4991=CARTESIAN_POINT('Ctrl Pts',(-1.6211138875,51.4229166676226,-0.935950539335166));
#4992=CARTESIAN_POINT('Ctrl Pts',(-0.81055694375,51.3645833342893,-1.40392580900275));
#4993=CARTESIAN_POINT('Ctrl Pts',(-1.14620883215705E-16,51.3062500009559,
-1.87190107867033));
#4994=CARTESIAN_POINT('Ctrl Pts',(0.81055694375,51.2479166676226,-1.40392580900275));
#4995=CARTESIAN_POINT('Ctrl Pts',(1.6211138875,51.1895833342892,-0.935950539335166));
#4996=CARTESIAN_POINT('Ctrl Pts',(1.6211138875,51.1312500009559,-1.9852919333802E-16));
#4997=CARTESIAN_POINT('Ctrl Pts',(1.6211138875,51.0729166676226,0.935950539335165));
#4998=CARTESIAN_POINT('Ctrl Pts',(0.810556943750001,51.0145833342893,1.40392580900275));
#4999=CARTESIAN_POINT('Ctrl Pts',(3.43862649647115E-16,50.9562500009559,
1.87190107867033));
#5000=CARTESIAN_POINT('Ctrl Pts',(-0.810556943749999,50.8979166676226,1.40392580900275));
#5001=CARTESIAN_POINT('Ctrl Pts',(-1.6211138875,50.8395833342893,0.935950539335167));
#5002=CARTESIAN_POINT('Ctrl Pts',(-1.6211138875,50.7812500009559,0.));
#5003=CARTESIAN_POINT('Ctrl Pts',(-1.6211138875,50.7229166676226,-0.935950539335166));
#5004=CARTESIAN_POINT('Ctrl Pts',(-0.81055694375,50.6645833342893,-1.40392580900275));
#5005=CARTESIAN_POINT('Ctrl Pts',(-1.14620883215705E-16,50.6062500009559,
-1.87190107867033));
#5006=CARTESIAN_POINT('Ctrl Pts',(0.81055694375,50.5479166676226,-1.40392580900275));
#5007=CARTESIAN_POINT('Ctrl Pts',(1.6211138875,50.4895833342893,-0.935950539335166));
#5008=CARTESIAN_POINT('Ctrl Pts',(1.6211138875,50.4312500009559,-1.9852919333802E-16));
#5009=CARTESIAN_POINT('Ctrl Pts',(1.6211138875,50.3729166676226,0.935950539335165));
#5010=CARTESIAN_POINT('Ctrl Pts',(0.810556943750001,50.3145833342893,1.40392580900275));
#5011=CARTESIAN_POINT('Ctrl Pts',(3.43862649647115E-16,50.2562500009559,
1.87190107867033));
#5012=CARTESIAN_POINT('Ctrl Pts',(-0.810556943749999,50.1979166676226,1.40392580900275));
#5013=CARTESIAN_POINT('Ctrl Pts',(-1.6211138875,50.1395833342892,0.935950539335167));
#5014=CARTESIAN_POINT('Ctrl Pts',(-1.6211138875,50.0812500009559,0.));
#5015=CARTESIAN_POINT('Ctrl Pts',(-1.6211138875,50.0229166676226,-0.935950539335166));
#5016=CARTESIAN_POINT('Ctrl Pts',(-0.81055694375,49.9645833342893,-1.40392580900275));
#5017=CARTESIAN_POINT('Ctrl Pts',(-1.14620883215705E-16,49.9062500009559,
-1.87190107867033));
#5018=CARTESIAN_POINT('Ctrl Pts',(0.81055694375,49.8479166676226,-1.40392580900275));
#5019=CARTESIAN_POINT('Ctrl Pts',(1.6211138875,49.7895833342893,-0.935950539335166));
#5020=CARTESIAN_POINT('Ctrl Pts',(1.6211138875,49.7312500009559,-1.9852919333802E-16));
#5021=CARTESIAN_POINT('Ctrl Pts',(1.6211138875,49.6729166676226,0.935950539335165));
#5022=CARTESIAN_POINT('Ctrl Pts',(0.810556943750001,49.6145833342893,1.40392580900275));
#5023=CARTESIAN_POINT('Ctrl Pts',(3.43862649647115E-16,49.5562500009559,
1.87190107867033));
#5024=CARTESIAN_POINT('Ctrl Pts',(-0.810556943749999,49.4979166676226,1.40392580900275));
#5025=CARTESIAN_POINT('Ctrl Pts',(-1.6211138875,49.4395833342893,0.935950539335167));
#5026=CARTESIAN_POINT('Ctrl Pts',(-1.6211138875,49.3812500009559,0.));
#5027=CARTESIAN_POINT('Ctrl Pts',(-1.6211138875,49.3229166676226,-0.935950539335166));
#5028=CARTESIAN_POINT('Ctrl Pts',(-0.81055694375,49.2645833342893,-1.40392580900275));
#5029=CARTESIAN_POINT('Ctrl Pts',(-1.14620883215705E-16,49.2062500009559,
-1.87190107867033));
#5030=CARTESIAN_POINT('Ctrl Pts',(0.81055694375,49.1479166676226,-1.40392580900275));
#5031=CARTESIAN_POINT('Ctrl Pts',(1.6211138875,49.0895833342893,-0.935950539335166));
#5032=CARTESIAN_POINT('Ctrl Pts',(1.6211138875,49.0312500009559,-1.9852919333802E-16));
#5033=CARTESIAN_POINT('Ctrl Pts',(1.6211138875,48.9729166676226,0.935950539335165));
#5034=CARTESIAN_POINT('Ctrl Pts',(0.810556943750001,48.9145833342893,1.40392580900275));
#5035=CARTESIAN_POINT('Ctrl Pts',(3.43862649647115E-16,48.8562500009559,
1.87190107867033));
#5036=CARTESIAN_POINT('Ctrl Pts',(-0.810556943749999,48.7979166676226,1.40392580900275));
#5037=CARTESIAN_POINT('Ctrl Pts',(-1.6211138875,48.7395833342893,0.935950539335167));
#5038=CARTESIAN_POINT('Ctrl Pts',(-1.6211138875,48.6812500009559,0.));
#5039=CARTESIAN_POINT('Ctrl Pts',(-1.6211138875,48.6229166676226,-0.935950539335166));
#5040=CARTESIAN_POINT('Ctrl Pts',(-0.81055694375,48.5645833342893,-1.40392580900275));
#5041=CARTESIAN_POINT('Ctrl Pts',(-1.14620883215705E-16,48.5062500009559,
-1.87190107867033));
#5042=CARTESIAN_POINT('Ctrl Pts',(0.81055694375,48.4479166676226,-1.40392580900275));
#5043=CARTESIAN_POINT('Ctrl Pts',(1.6211138875,48.3895833342893,-0.935950539335166));
#5044=CARTESIAN_POINT('Ctrl Pts',(1.6211138875,48.3312500009559,-1.9852919333802E-16));
#5045=CARTESIAN_POINT('Ctrl Pts',(1.6211138875,48.2729166676226,0.935950539335165));
#5046=CARTESIAN_POINT('Ctrl Pts',(0.810556943750001,48.2145833342893,1.40392580900275));
#5047=CARTESIAN_POINT('Ctrl Pts',(3.43862649647115E-16,48.1562500009559,
1.87190107867033));
#5048=CARTESIAN_POINT('Ctrl Pts',(-0.810556943749999,48.0979166676226,1.40392580900275));
#5049=CARTESIAN_POINT('Ctrl Pts',(-1.6211138875,48.0395833342893,0.935950539335167));
#5050=CARTESIAN_POINT('Ctrl Pts',(-1.6211138875,47.9812500009559,0.));
#5051=CARTESIAN_POINT('Ctrl Pts',(-1.6211138875,47.9229166676226,-0.935950539335166));
#5052=CARTESIAN_POINT('Ctrl Pts',(-0.81055694375,47.8645833342893,-1.40392580900275));
#5053=CARTESIAN_POINT('Ctrl Pts',(-1.14620883215705E-16,47.8062500009559,
-1.87190107867033));
#5054=CARTESIAN_POINT('Ctrl Pts',(0.81055694375,47.7479166676226,-1.40392580900275));
#5055=CARTESIAN_POINT('Ctrl Pts',(1.6211138875,47.6895833342893,-0.935950539335166));
#5056=CARTESIAN_POINT('Ctrl Pts',(1.6211138875,47.6312500009559,-1.9852919333802E-16));
#5057=CARTESIAN_POINT('Ctrl Pts',(1.6211138875,47.5729166676226,0.935950539335165));
#5058=CARTESIAN_POINT('Ctrl Pts',(0.810556943750001,47.5145833342893,1.40392580900275));
#5059=CARTESIAN_POINT('Ctrl Pts',(3.43862649647115E-16,47.4562500009559,
1.87190107867033));
#5060=CARTESIAN_POINT('Ctrl Pts',(-0.810556943749999,47.3979166676226,1.40392580900275));
#5061=CARTESIAN_POINT('Ctrl Pts',(-1.6211138875,47.3395833342893,0.935950539335167));
#5062=CARTESIAN_POINT('Ctrl Pts',(-1.6211138875,47.2812500009559,0.));
#5063=CARTESIAN_POINT('Ctrl Pts',(-1.6211138875,47.2229166676226,-0.935950539335166));
#5064=CARTESIAN_POINT('Ctrl Pts',(-0.81055694375,47.1645833342893,-1.40392580900275));
#5065=CARTESIAN_POINT('Ctrl Pts',(-1.14620883215705E-16,47.1062500009559,
-1.87190107867033));
#5066=CARTESIAN_POINT('Ctrl Pts',(0.81055694375,47.0479166676226,-1.40392580900275));
#5067=CARTESIAN_POINT('Ctrl Pts',(1.6211138875,46.9895833342893,-0.935950539335166));
#5068=CARTESIAN_POINT('Ctrl Pts',(1.6211138875,46.9312500009559,-1.9852919333802E-16));
#5069=CARTESIAN_POINT('Ctrl Pts',(1.6211138875,46.8729166676226,0.935950539335165));
#5070=CARTESIAN_POINT('Ctrl Pts',(0.810556943750001,46.8145833342893,1.40392580900275));
#5071=CARTESIAN_POINT('Ctrl Pts',(3.43862649647115E-16,46.7562500009559,
1.87190107867033));
#5072=CARTESIAN_POINT('Ctrl Pts',(-0.810556943749999,46.6979166676226,1.40392580900275));
#5073=CARTESIAN_POINT('Ctrl Pts',(-1.6211138875,46.6395833342893,0.935950539335167));
#5074=CARTESIAN_POINT('Ctrl Pts',(-1.6211138875,46.5812500009559,0.));
#5075=CARTESIAN_POINT('Ctrl Pts',(-1.6211138875,46.5229166676226,-0.935950539335166));
#5076=CARTESIAN_POINT('Ctrl Pts',(-0.81055694375,46.4645833342893,-1.40392580900275));
#5077=CARTESIAN_POINT('Ctrl Pts',(-1.14620883215705E-16,46.4062500009559,
-1.87190107867033));
#5078=CARTESIAN_POINT('Ctrl Pts',(0.81055694375,46.3479166676226,-1.40392580900275));
#5079=CARTESIAN_POINT('Ctrl Pts',(1.6211138875,46.2895833342893,-0.935950539335166));
#5080=CARTESIAN_POINT('Ctrl Pts',(1.6211138875,46.2312500009559,-1.9852919333802E-16));
#5081=CARTESIAN_POINT('Ctrl Pts',(1.6211138875,46.1729166676226,0.935950539335165));
#5082=CARTESIAN_POINT('Ctrl Pts',(0.810556943750001,46.1145833342893,1.40392580900275));
#5083=CARTESIAN_POINT('Ctrl Pts',(3.43862649647115E-16,46.0562500009559,
1.87190107867033));
#5084=CARTESIAN_POINT('Ctrl Pts',(-0.810556943749999,45.9979166676226,1.40392580900275));
#5085=CARTESIAN_POINT('Ctrl Pts',(-1.6211138875,45.9395833342893,0.935950539335167));
#5086=CARTESIAN_POINT('Ctrl Pts',(-1.6211138875,45.8812500009559,0.));
#5087=CARTESIAN_POINT('Ctrl Pts',(-1.6211138875,45.8229166676226,-0.935950539335166));
#5088=CARTESIAN_POINT('Ctrl Pts',(-0.81055694375,45.7645833342893,-1.40392580900275));
#5089=CARTESIAN_POINT('Ctrl Pts',(-1.14620883215705E-16,45.7062500009559,
-1.87190107867033));
#5090=CARTESIAN_POINT('Ctrl Pts',(0.81055694375,45.6479166676226,-1.40392580900275));
#5091=CARTESIAN_POINT('Ctrl Pts',(1.6211138875,45.5895833342893,-0.935950539335166));
#5092=CARTESIAN_POINT('Ctrl Pts',(1.6211138875,45.5312500009559,-1.9852919333802E-16));
#5093=CARTESIAN_POINT('Ctrl Pts',(1.6211138875,45.4729166676226,0.935950539335165));
#5094=CARTESIAN_POINT('Ctrl Pts',(0.810556943750001,45.4145833342893,1.40392580900275));
#5095=CARTESIAN_POINT('Ctrl Pts',(3.43862649647115E-16,45.3562500009559,
1.87190107867033));
#5096=CARTESIAN_POINT('Ctrl Pts',(-0.810556943749999,45.2979166676226,1.40392580900275));
#5097=CARTESIAN_POINT('Ctrl Pts',(-1.6211138875,45.2395833342893,0.935950539335167));
#5098=CARTESIAN_POINT('Ctrl Pts',(-1.6211138875,45.1812500009559,0.));
#5099=CARTESIAN_POINT('Ctrl Pts',(-1.6211138875,45.1229166676226,-0.935950539335166));
#5100=CARTESIAN_POINT('Ctrl Pts',(-0.81055694375,45.0645833342893,-1.40392580900275));
#5101=CARTESIAN_POINT('Ctrl Pts',(-1.14620883215705E-16,45.0062500009559,
-1.87190107867033));
#5102=CARTESIAN_POINT('Ctrl Pts',(0.81055694375,44.9479166676226,-1.40392580900275));
#5103=CARTESIAN_POINT('Ctrl Pts',(1.6211138875,44.8895833342893,-0.935950539335166));
#5104=CARTESIAN_POINT('Ctrl Pts',(1.6211138875,44.8312500009559,-1.9852919333802E-16));
#5105=CARTESIAN_POINT('Ctrl Pts',(1.6211138875,44.7729166676226,0.935950539335165));
#5106=CARTESIAN_POINT('Ctrl Pts',(0.810556943750001,44.7145833342893,1.40392580900275));
#5107=CARTESIAN_POINT('Ctrl Pts',(3.43862649647115E-16,44.6562500009559,
1.87190107867033));
#5108=CARTESIAN_POINT('Ctrl Pts',(-0.810556943749999,44.5979166676226,1.40392580900275));
#5109=CARTESIAN_POINT('Ctrl Pts',(-1.6211138875,44.5395833342893,0.935950539335167));
#5110=CARTESIAN_POINT('Ctrl Pts',(-1.6211138875,44.4812500009559,0.));
#5111=CARTESIAN_POINT('Ctrl Pts',(-1.6211138875,44.4229166676226,-0.935950539335166));
#5112=CARTESIAN_POINT('Ctrl Pts',(-0.81055694375,44.3645833342893,-1.40392580900275));
#5113=CARTESIAN_POINT('Ctrl Pts',(-1.14620883215705E-16,44.3062500009559,
-1.87190107867033));
#5114=CARTESIAN_POINT('Ctrl Pts',(0.81055694375,44.2479166676226,-1.40392580900275));
#5115=CARTESIAN_POINT('Ctrl Pts',(1.6211138875,44.1895833342893,-0.935950539335166));
#5116=CARTESIAN_POINT('Ctrl Pts',(1.6211138875,44.1312500009559,-1.9852919333802E-16));
#5117=CARTESIAN_POINT('Ctrl Pts',(1.6211138875,44.0729166676226,0.935950539335165));
#5118=CARTESIAN_POINT('Ctrl Pts',(0.810556943750001,44.0145833342893,1.40392580900275));
#5119=CARTESIAN_POINT('Ctrl Pts',(3.43862649647115E-16,43.9562500009559,
1.87190107867033));
#5120=CARTESIAN_POINT('Ctrl Pts',(-0.810556943749999,43.8979166676226,1.40392580900275));
#5121=CARTESIAN_POINT('Ctrl Pts',(-1.6211138875,43.8395833342893,0.935950539335167));
#5122=CARTESIAN_POINT('Ctrl Pts',(-1.6211138875,43.7812500009559,0.));
#5123=CARTESIAN_POINT('Ctrl Pts',(-1.6211138875,43.7229166676226,-0.935950539335166));
#5124=CARTESIAN_POINT('Ctrl Pts',(-0.81055694375,43.6645833342893,-1.40392580900275));
#5125=CARTESIAN_POINT('Ctrl Pts',(-1.14620883215705E-16,43.6062500009559,
-1.87190107867033));
#5126=CARTESIAN_POINT('Ctrl Pts',(0.81055694375,43.5479166676226,-1.40392580900275));
#5127=CARTESIAN_POINT('Ctrl Pts',(1.6211138875,43.4895833342893,-0.935950539335166));
#5128=CARTESIAN_POINT('Ctrl Pts',(1.6211138875,43.4312500009559,-1.9852919333802E-16));
#5129=CARTESIAN_POINT('Ctrl Pts',(1.6211138875,43.3729166676226,0.935950539335165));
#5130=CARTESIAN_POINT('Ctrl Pts',(0.810556943750001,43.3145833342893,1.40392580900275));
#5131=CARTESIAN_POINT('Ctrl Pts',(3.43862649647115E-16,43.2562500009559,
1.87190107867033));
#5132=CARTESIAN_POINT('Ctrl Pts',(-0.810556943749999,43.1979166676226,1.40392580900275));
#5133=CARTESIAN_POINT('Ctrl Pts',(-1.6211138875,43.1395833342893,0.935950539335167));
#5134=CARTESIAN_POINT('Ctrl Pts',(-1.6211138875,43.0812500009559,0.));
#5135=CARTESIAN_POINT('Ctrl Pts',(-1.6211138875,43.0229166676226,-0.935950539335166));
#5136=CARTESIAN_POINT('Ctrl Pts',(-0.81055694375,42.9645833342893,-1.40392580900275));
#5137=CARTESIAN_POINT('Ctrl Pts',(-1.14620883215705E-16,42.9062500009559,
-1.87190107867033));
#5138=CARTESIAN_POINT('Ctrl Pts',(0.81055694375,42.8479166676226,-1.40392580900275));
#5139=CARTESIAN_POINT('Ctrl Pts',(1.6211138875,42.7895833342893,-0.935950539335166));
#5140=CARTESIAN_POINT('Ctrl Pts',(1.6211138875,42.7312500009559,-1.9852919333802E-16));
#5141=CARTESIAN_POINT('Ctrl Pts',(1.6211138875,42.6729166676226,0.935950539335165));
#5142=CARTESIAN_POINT('Ctrl Pts',(0.810556943750001,42.6145833342893,1.40392580900275));
#5143=CARTESIAN_POINT('Ctrl Pts',(3.43862649647115E-16,42.5562500009559,
1.87190107867033));
#5144=CARTESIAN_POINT('Ctrl Pts',(-0.810556943749999,42.4979166676226,1.40392580900275));
#5145=CARTESIAN_POINT('Ctrl Pts',(-1.6211138875,42.4395833342892,0.935950539335167));
#5146=CARTESIAN_POINT('Ctrl Pts',(-1.6211138875,42.3812500009559,0.));
#5147=CARTESIAN_POINT('Ctrl Pts',(-1.6211138875,42.3229166676226,-0.935950539335166));
#5148=CARTESIAN_POINT('Ctrl Pts',(-0.81055694375,42.2645833342893,-1.40392580900275));
#5149=CARTESIAN_POINT('Ctrl Pts',(-1.14620883215705E-16,42.2062500009559,
-1.87190107867033));
#5150=CARTESIAN_POINT('Ctrl Pts',(0.81055694375,42.1479166676226,-1.40392580900275));
#5151=CARTESIAN_POINT('Ctrl Pts',(1.6211138875,42.0895833342893,-0.935950539335166));
#5152=CARTESIAN_POINT('Ctrl Pts',(1.6211138875,42.0312500009559,-1.9852919333802E-16));
#5153=CARTESIAN_POINT('Ctrl Pts',(1.6211138875,41.9729166676226,0.935950539335165));
#5154=CARTESIAN_POINT('Ctrl Pts',(0.810556943750001,41.9145833342893,1.40392580900275));
#5155=CARTESIAN_POINT('Ctrl Pts',(3.43862649647115E-16,41.8562500009559,
1.87190107867033));
#5156=CARTESIAN_POINT('Ctrl Pts',(-0.810556943749999,41.7979166676226,1.40392580900275));
#5157=CARTESIAN_POINT('Ctrl Pts',(-1.6211138875,41.7395833342893,0.935950539335167));
#5158=CARTESIAN_POINT('Ctrl Pts',(-1.6211138875,41.6812500009559,0.));
#5159=CARTESIAN_POINT('Ctrl Pts',(-1.6211138875,41.6229166676226,-0.935950539335166));
#5160=CARTESIAN_POINT('Ctrl Pts',(-0.81055694375,41.5645833342893,-1.40392580900275));
#5161=CARTESIAN_POINT('Ctrl Pts',(-1.14620883215705E-16,41.5062500009559,
-1.87190107867033));
#5162=CARTESIAN_POINT('Ctrl Pts',(0.81055694375,41.4479166676226,-1.40392580900275));
#5163=CARTESIAN_POINT('Ctrl Pts',(1.6211138875,41.3895833342893,-0.935950539335166));
#5164=CARTESIAN_POINT('Ctrl Pts',(1.6211138875,41.3312500009559,-1.9852919333802E-16));
#5165=CARTESIAN_POINT('Ctrl Pts',(1.6211138875,41.2729166676226,0.935950539335165));
#5166=CARTESIAN_POINT('Ctrl Pts',(0.810556943750001,41.2145833342893,1.40392580900275));
#5167=CARTESIAN_POINT('Ctrl Pts',(3.43862649647115E-16,41.1562500009559,
1.87190107867033));
#5168=CARTESIAN_POINT('Ctrl Pts',(-0.810556943749999,41.0979166676226,1.40392580900275));
#5169=CARTESIAN_POINT('Ctrl Pts',(-1.6211138875,41.0395833342892,0.935950539335167));
#5170=CARTESIAN_POINT('Ctrl Pts',(-1.6211138875,40.9812500009559,0.));
#5171=CARTESIAN_POINT('Ctrl Pts',(-1.6211138875,40.9229166676226,-0.935950539335166));
#5172=CARTESIAN_POINT('Ctrl Pts',(-0.81055694375,40.8645833342893,-1.40392580900275));
#5173=CARTESIAN_POINT('Ctrl Pts',(-1.14620883215705E-16,40.8062500009559,
-1.87190107867033));
#5174=CARTESIAN_POINT('Ctrl Pts',(0.81055694375,40.7479166676226,-1.40392580900275));
#5175=CARTESIAN_POINT('Ctrl Pts',(1.6211138875,40.6895833342893,-0.935950539335166));
#5176=CARTESIAN_POINT('Ctrl Pts',(1.6211138875,40.6312500009559,-1.9852919333802E-16));
#5177=CARTESIAN_POINT('Ctrl Pts',(1.6211138875,40.5729166676226,0.935950539335165));
#5178=CARTESIAN_POINT('Ctrl Pts',(0.810556943750001,40.5145833342893,1.40392580900275));
#5179=CARTESIAN_POINT('Ctrl Pts',(3.43862649647115E-16,40.4562500009559,
1.87190107867033));
#5180=CARTESIAN_POINT('Ctrl Pts',(-0.810556943749999,40.3979166676226,1.40392580900275));
#5181=CARTESIAN_POINT('Ctrl Pts',(-1.6211138875,40.3395833342893,0.935950539335167));
#5182=CARTESIAN_POINT('Ctrl Pts',(-1.6211138875,40.2812500009559,0.));
#5183=CARTESIAN_POINT('Ctrl Pts',(-1.6211138875,40.2229166676226,-0.935950539335166));
#5184=CARTESIAN_POINT('Ctrl Pts',(-0.81055694375,40.1645833342893,-1.40392580900275));
#5185=CARTESIAN_POINT('Ctrl Pts',(-1.14620883215705E-16,40.1062500009559,
-1.87190107867033));
#5186=CARTESIAN_POINT('Ctrl Pts',(0.81055694375,40.0479166676226,-1.40392580900275));
#5187=CARTESIAN_POINT('Ctrl Pts',(1.6211138875,39.9895833342893,-0.935950539335166));
#5188=CARTESIAN_POINT('Ctrl Pts',(1.6211138875,39.9312500009559,-1.9852919333802E-16));
#5189=CARTESIAN_POINT('Ctrl Pts',(1.6211138875,39.8729166676226,0.935950539335165));
#5190=CARTESIAN_POINT('Ctrl Pts',(0.810556943750001,39.8145833342893,1.40392580900275));
#5191=CARTESIAN_POINT('Ctrl Pts',(3.43862649647115E-16,39.7562500009559,
1.87190107867033));
#5192=CARTESIAN_POINT('Ctrl Pts',(-0.810556943749999,39.6979166676226,1.40392580900275));
#5193=CARTESIAN_POINT('Ctrl Pts',(-1.6211138875,39.6395833342893,0.935950539335167));
#5194=CARTESIAN_POINT('Ctrl Pts',(-1.6211138875,39.5812500009559,0.));
#5195=CARTESIAN_POINT('Ctrl Pts',(-1.6211138875,39.5229166676226,-0.935950539335166));
#5196=CARTESIAN_POINT('Ctrl Pts',(-0.81055694375,39.4645833342893,-1.40392580900275));
#5197=CARTESIAN_POINT('Ctrl Pts',(-1.14620883215705E-16,39.4062500009559,
-1.87190107867033));
#5198=CARTESIAN_POINT('Ctrl Pts',(0.81055694375,39.3479166676226,-1.40392580900275));
#5199=CARTESIAN_POINT('Ctrl Pts',(1.6211138875,39.2895833342892,-0.935950539335166));
#5200=CARTESIAN_POINT('Ctrl Pts',(1.6211138875,39.2312500009559,-1.9852919333802E-16));
#5201=CARTESIAN_POINT('Ctrl Pts',(1.6211138875,39.1729166676226,0.935950539335165));
#5202=CARTESIAN_POINT('Ctrl Pts',(0.810556943750001,39.1145833342893,1.40392580900275));
#5203=CARTESIAN_POINT('Ctrl Pts',(3.43862649647115E-16,39.0562500009559,
1.87190107867033));
#5204=CARTESIAN_POINT('Ctrl Pts',(-0.810556943749999,38.9979166676226,1.40392580900275));
#5205=CARTESIAN_POINT('Ctrl Pts',(-1.6211138875,38.9395833342893,0.935950539335167));
#5206=CARTESIAN_POINT('Ctrl Pts',(-1.6211138875,38.8812500009559,0.));
#5207=CARTESIAN_POINT('Ctrl Pts',(-1.6211138875,38.8229166676226,-0.935950539335166));
#5208=CARTESIAN_POINT('Ctrl Pts',(-0.81055694375,38.7645833342893,-1.40392580900275));
#5209=CARTESIAN_POINT('Ctrl Pts',(-1.14620883215705E-16,38.7062500009559,
-1.87190107867033));
#5210=CARTESIAN_POINT('Ctrl Pts',(0.81055694375,38.6479166676226,-1.40392580900275));
#5211=CARTESIAN_POINT('Ctrl Pts',(1.6211138875,38.5895833342893,-0.935950539335166));
#5212=CARTESIAN_POINT('Ctrl Pts',(1.6211138875,38.5312500009559,-1.9852919333802E-16));
#5213=CARTESIAN_POINT('Ctrl Pts',(1.6211138875,38.4729166676226,0.935950539335165));
#5214=CARTESIAN_POINT('Ctrl Pts',(0.810556943750001,38.4145833342893,1.40392580900275));
#5215=CARTESIAN_POINT('Ctrl Pts',(3.43862649647115E-16,38.3562500009559,
1.87190107867033));
#5216=CARTESIAN_POINT('Ctrl Pts',(-0.810556943749999,38.2979166676226,1.40392580900275));
#5217=CARTESIAN_POINT('Ctrl Pts',(-1.6211138875,38.2395833342893,0.935950539335167));
#5218=CARTESIAN_POINT('Ctrl Pts',(-1.6211138875,38.1812500009559,0.));
#5219=CARTESIAN_POINT('Ctrl Pts',(-1.6211138875,38.1229166676226,-0.935950539335166));
#5220=CARTESIAN_POINT('Ctrl Pts',(-0.81055694375,38.0645833342893,-1.40392580900275));
#5221=CARTESIAN_POINT('Ctrl Pts',(-1.14620883215705E-16,38.0062500009559,
-1.87190107867033));
#5222=CARTESIAN_POINT('Ctrl Pts',(0.81055694375,37.9479166676226,-1.40392580900275));
#5223=CARTESIAN_POINT('Ctrl Pts',(1.6211138875,37.8895833342893,-0.935950539335166));
#5224=CARTESIAN_POINT('Ctrl Pts',(1.6211138875,37.8312500009559,-1.9852919333802E-16));
#5225=CARTESIAN_POINT('Ctrl Pts',(1.6211138875,37.7729166676226,0.935950539335165));
#5226=CARTESIAN_POINT('Ctrl Pts',(0.810556943750001,37.7145833342893,1.40392580900275));
#5227=CARTESIAN_POINT('Ctrl Pts',(3.43862649647115E-16,37.6562500009559,
1.87190107867033));
#5228=CARTESIAN_POINT('Ctrl Pts',(-0.810556943749999,37.5979166676226,1.40392580900275));
#5229=CARTESIAN_POINT('Ctrl Pts',(-1.6211138875,37.5395833342893,0.935950539335167));
#5230=CARTESIAN_POINT('Ctrl Pts',(-1.6211138875,37.4812500009559,0.));
#5231=CARTESIAN_POINT('Ctrl Pts',(-1.6211138875,37.4229166676226,-0.935950539335166));
#5232=CARTESIAN_POINT('Ctrl Pts',(-0.81055694375,37.3645833342893,-1.40392580900275));
#5233=CARTESIAN_POINT('Ctrl Pts',(-1.14620883215705E-16,37.3062500009559,
-1.87190107867033));
#5234=CARTESIAN_POINT('Ctrl Pts',(0.81055694375,37.2479166676226,-1.40392580900275));
#5235=CARTESIAN_POINT('Ctrl Pts',(1.6211138875,37.1895833342893,-0.935950539335166));
#5236=CARTESIAN_POINT('Ctrl Pts',(1.6211138875,37.1312500009559,-1.9852919333802E-16));
#5237=CARTESIAN_POINT('Ctrl Pts',(1.6211138875,37.0729166676226,0.935950539335165));
#5238=CARTESIAN_POINT('Ctrl Pts',(0.810556943750001,37.0145833342893,1.40392580900275));
#5239=CARTESIAN_POINT('Ctrl Pts',(3.43862649647115E-16,36.9562500009559,
1.87190107867033));
#5240=CARTESIAN_POINT('Ctrl Pts',(-0.810556943749999,36.8979166676226,1.40392580900275));
#5241=CARTESIAN_POINT('Ctrl Pts',(-1.6211138875,36.8395833342893,0.935950539335167));
#5242=CARTESIAN_POINT('Ctrl Pts',(-1.6211138875,36.7812500009559,0.));
#5243=CARTESIAN_POINT('Ctrl Pts',(-1.6211138875,36.7229166676226,-0.935950539335166));
#5244=CARTESIAN_POINT('Ctrl Pts',(-0.81055694375,36.6645833342893,-1.40392580900275));
#5245=CARTESIAN_POINT('Ctrl Pts',(-1.14620883215705E-16,36.6062500009559,
-1.87190107867033));
#5246=CARTESIAN_POINT('Ctrl Pts',(0.81055694375,36.5479166676226,-1.40392580900275));
#5247=CARTESIAN_POINT('Ctrl Pts',(1.6211138875,36.4895833342893,-0.935950539335166));
#5248=CARTESIAN_POINT('Ctrl Pts',(1.6211138875,36.4312500009559,-1.9852919333802E-16));
#5249=CARTESIAN_POINT('Ctrl Pts',(1.6211138875,36.3729166676226,0.935950539335165));
#5250=CARTESIAN_POINT('Ctrl Pts',(0.810556943750001,36.3145833342893,1.40392580900275));
#5251=CARTESIAN_POINT('Ctrl Pts',(3.43862649647115E-16,36.2562500009559,
1.87190107867033));
#5252=CARTESIAN_POINT('Ctrl Pts',(-0.810556943749999,36.1979166676226,1.40392580900275));
#5253=CARTESIAN_POINT('Ctrl Pts',(-1.6211138875,36.1395833342893,0.935950539335167));
#5254=CARTESIAN_POINT('Ctrl Pts',(-1.6211138875,36.0812500009559,0.));
#5255=CARTESIAN_POINT('Ctrl Pts',(-1.6211138875,36.0229166676226,-0.935950539335166));
#5256=CARTESIAN_POINT('Ctrl Pts',(-0.81055694375,35.9645833342893,-1.40392580900275));
#5257=CARTESIAN_POINT('Ctrl Pts',(-1.14620883215705E-16,35.9062500009559,
-1.87190107867033));
#5258=CARTESIAN_POINT('Ctrl Pts',(0.81055694375,35.8479166676226,-1.40392580900275));
#5259=CARTESIAN_POINT('Ctrl Pts',(1.6211138875,35.7895833342893,-0.935950539335166));
#5260=CARTESIAN_POINT('Ctrl Pts',(1.6211138875,35.7312500009559,-1.9852919333802E-16));
#5261=CARTESIAN_POINT('Ctrl Pts',(1.6211138875,35.6729166676226,0.935950539335165));
#5262=CARTESIAN_POINT('Ctrl Pts',(0.810556943750001,35.6145833342893,1.40392580900275));
#5263=CARTESIAN_POINT('Ctrl Pts',(3.43862649647115E-16,35.5562500009559,
1.87190107867033));
#5264=CARTESIAN_POINT('Ctrl Pts',(-0.810556943749999,35.4979166676226,1.40392580900275));
#5265=CARTESIAN_POINT('Ctrl Pts',(-1.6211138875,35.4395833342893,0.935950539335167));
#5266=CARTESIAN_POINT('Ctrl Pts',(-1.6211138875,35.3812500009559,0.));
#5267=CARTESIAN_POINT('Ctrl Pts',(-1.6211138875,35.3229166676226,-0.935950539335166));
#5268=CARTESIAN_POINT('Ctrl Pts',(-0.81055694375,35.2645833342893,-1.40392580900275));
#5269=CARTESIAN_POINT('Ctrl Pts',(-1.14620883215705E-16,35.2062500009559,
-1.87190107867033));
#5270=CARTESIAN_POINT('Ctrl Pts',(0.81055694375,35.1479166676226,-1.40392580900275));
#5271=CARTESIAN_POINT('Ctrl Pts',(1.6211138875,35.0895833342893,-0.935950539335166));
#5272=CARTESIAN_POINT('Ctrl Pts',(1.6211138875,35.0312500009559,-1.9852919333802E-16));
#5273=CARTESIAN_POINT('Ctrl Pts',(1.6211138875,34.9729166676226,0.935950539335165));
#5274=CARTESIAN_POINT('Ctrl Pts',(0.810556943750001,34.9145833342893,1.40392580900275));
#5275=CARTESIAN_POINT('Ctrl Pts',(3.43862649647115E-16,34.8562500009559,
1.87190107867033));
#5276=CARTESIAN_POINT('Ctrl Pts',(-0.810556943749999,34.7979166676226,1.40392580900275));
#5277=CARTESIAN_POINT('Ctrl Pts',(-1.6211138875,34.7395833342893,0.935950539335167));
#5278=CARTESIAN_POINT('Ctrl Pts',(-1.6211138875,34.6812500009559,0.));
#5279=CARTESIAN_POINT('Ctrl Pts',(-1.6211138875,34.6229166676226,-0.935950539335166));
#5280=CARTESIAN_POINT('Ctrl Pts',(-0.81055694375,34.5645833342893,-1.40392580900275));
#5281=CARTESIAN_POINT('Ctrl Pts',(-1.14620883215705E-16,34.5062500009559,
-1.87190107867033));
#5282=CARTESIAN_POINT('Ctrl Pts',(0.81055694375,34.4479166676226,-1.40392580900275));
#5283=CARTESIAN_POINT('Ctrl Pts',(1.6211138875,34.3895833342893,-0.935950539335166));
#5284=CARTESIAN_POINT('Ctrl Pts',(1.6211138875,34.3312500009559,-1.9852919333802E-16));
#5285=CARTESIAN_POINT('Ctrl Pts',(1.6211138875,34.2729166676226,0.935950539335165));
#5286=CARTESIAN_POINT('Ctrl Pts',(0.810556943750001,34.2145833342893,1.40392580900275));
#5287=CARTESIAN_POINT('Ctrl Pts',(3.43862649647115E-16,34.1562500009559,
1.87190107867033));
#5288=CARTESIAN_POINT('Ctrl Pts',(-0.810556943749999,34.0979166676226,1.40392580900275));
#5289=CARTESIAN_POINT('Ctrl Pts',(-1.6211138875,34.0395833342892,0.935950539335167));
#5290=CARTESIAN_POINT('Ctrl Pts',(-1.6211138875,33.9812500009559,0.));
#5291=CARTESIAN_POINT('Ctrl Pts',(-1.6211138875,33.9229166676226,-0.935950539335166));
#5292=CARTESIAN_POINT('Ctrl Pts',(-0.81055694375,33.8645833342893,-1.40392580900275));
#5293=CARTESIAN_POINT('Ctrl Pts',(-1.14620883215705E-16,33.8062500009559,
-1.87190107867033));
#5294=CARTESIAN_POINT('Ctrl Pts',(0.81055694375,33.7479166676226,-1.40392580900275));
#5295=CARTESIAN_POINT('Ctrl Pts',(1.6211138875,33.6895833342892,-0.935950539335166));
#5296=CARTESIAN_POINT('Ctrl Pts',(1.6211138875,33.6312500009559,-1.9852919333802E-16));
#5297=CARTESIAN_POINT('Ctrl Pts',(1.6211138875,33.5729166676226,0.935950539335165));
#5298=CARTESIAN_POINT('Ctrl Pts',(0.810556943750001,33.5145833342893,1.40392580900275));
#5299=CARTESIAN_POINT('Ctrl Pts',(3.43862649647115E-16,33.4562500009559,
1.87190107867033));
#5300=CARTESIAN_POINT('Ctrl Pts',(-0.810556943749999,33.3979166676226,1.40392580900275));
#5301=CARTESIAN_POINT('Ctrl Pts',(-1.6211138875,33.3395833342893,0.935950539335167));
#5302=CARTESIAN_POINT('Ctrl Pts',(-1.6211138875,33.2812500009559,0.));
#5303=CARTESIAN_POINT('Ctrl Pts',(-1.6211138875,33.2229166676226,-0.935950539335166));
#5304=CARTESIAN_POINT('Ctrl Pts',(-0.81055694375,33.1645833342893,-1.40392580900275));
#5305=CARTESIAN_POINT('Ctrl Pts',(-1.14620883215705E-16,33.1062500009559,
-1.87190107867033));
#5306=CARTESIAN_POINT('Ctrl Pts',(0.81055694375,33.0479166676226,-1.40392580900275));
#5307=CARTESIAN_POINT('Ctrl Pts',(1.6211138875,32.9895833342893,-0.935950539335166));
#5308=CARTESIAN_POINT('Ctrl Pts',(1.6211138875,32.9312500009559,-1.9852919333802E-16));
#5309=CARTESIAN_POINT('Ctrl Pts',(1.6211138875,32.8729166676226,0.935950539335165));
#5310=CARTESIAN_POINT('Ctrl Pts',(0.810556943750001,32.8145833342893,1.40392580900275));
#5311=CARTESIAN_POINT('Ctrl Pts',(3.43862649647115E-16,32.7562500009559,
1.87190107867033));
#5312=CARTESIAN_POINT('Ctrl Pts',(-0.810556943749999,32.6979166676226,1.40392580900275));
#5313=CARTESIAN_POINT('Ctrl Pts',(-1.6211138875,32.6395833342893,0.935950539335167));
#5314=CARTESIAN_POINT('Ctrl Pts',(-1.6211138875,32.5812500009559,0.));
#5315=CARTESIAN_POINT('Ctrl Pts',(-1.6211138875,32.5229166676226,-0.935950539335166));
#5316=CARTESIAN_POINT('Ctrl Pts',(-0.81055694375,32.4645833342893,-1.40392580900275));
#5317=CARTESIAN_POINT('Ctrl Pts',(-1.14620883215705E-16,32.4062500009559,
-1.87190107867033));
#5318=CARTESIAN_POINT('Ctrl Pts',(0.81055694375,32.3479166676226,-1.40392580900275));
#5319=CARTESIAN_POINT('Ctrl Pts',(1.6211138875,32.2895833342893,-0.935950539335166));
#5320=CARTESIAN_POINT('Ctrl Pts',(1.6211138875,32.2312500009559,-1.9852919333802E-16));
#5321=CARTESIAN_POINT('Ctrl Pts',(1.6211138875,32.1729166676226,0.935950539335165));
#5322=CARTESIAN_POINT('Ctrl Pts',(0.810556943750001,32.1145833342893,1.40392580900275));
#5323=CARTESIAN_POINT('Ctrl Pts',(3.43862649647115E-16,32.0562500009559,
1.87190107867033));
#5324=CARTESIAN_POINT('Ctrl Pts',(-0.810556943749999,31.9979166676226,1.40392580900275));
#5325=CARTESIAN_POINT('Ctrl Pts',(-1.6211138875,31.9395833342893,0.935950539335167));
#5326=CARTESIAN_POINT('Ctrl Pts',(-1.6211138875,31.8812500009559,0.));
#5327=CARTESIAN_POINT('Ctrl Pts',(-1.6211138875,31.8229166676226,-0.935950539335166));
#5328=CARTESIAN_POINT('Ctrl Pts',(-0.81055694375,31.7645833342893,-1.40392580900275));
#5329=CARTESIAN_POINT('Ctrl Pts',(-1.14620883215705E-16,31.7062500009559,
-1.87190107867033));
#5330=CARTESIAN_POINT('Ctrl Pts',(0.81055694375,31.6479166676226,-1.40392580900275));
#5331=CARTESIAN_POINT('Ctrl Pts',(1.6211138875,31.5895833342893,-0.935950539335166));
#5332=CARTESIAN_POINT('Ctrl Pts',(1.6211138875,31.5312500009559,-1.9852919333802E-16));
#5333=CARTESIAN_POINT('Ctrl Pts',(1.6211138875,31.4729166676226,0.935950539335165));
#5334=CARTESIAN_POINT('Ctrl Pts',(0.810556943750001,31.4145833342893,1.40392580900275));
#5335=CARTESIAN_POINT('Ctrl Pts',(3.43862649647115E-16,31.3562500009559,
1.87190107867033));
#5336=CARTESIAN_POINT('Ctrl Pts',(-0.810556943749999,31.2979166676226,1.40392580900275));
#5337=CARTESIAN_POINT('Ctrl Pts',(-1.6211138875,31.2395833342893,0.935950539335167));
#5338=CARTESIAN_POINT('Ctrl Pts',(-1.6211138875,31.1812500009559,0.));
#5339=CARTESIAN_POINT('Ctrl Pts',(-1.6211138875,31.1229166676226,-0.935950539335166));
#5340=CARTESIAN_POINT('Ctrl Pts',(-0.81055694375,31.0645833342893,-1.40392580900275));
#5341=CARTESIAN_POINT('Ctrl Pts',(-1.14620883215705E-16,31.0062500009559,
-1.87190107867033));
#5342=CARTESIAN_POINT('Ctrl Pts',(0.81055694375,30.9479166676226,-1.40392580900275));
#5343=CARTESIAN_POINT('Ctrl Pts',(1.6211138875,30.8895833342893,-0.935950539335166));
#5344=CARTESIAN_POINT('Ctrl Pts',(1.6211138875,30.8312500009559,-1.9852919333802E-16));
#5345=CARTESIAN_POINT('Ctrl Pts',(1.6211138875,30.7729166676226,0.935950539335165));
#5346=CARTESIAN_POINT('Ctrl Pts',(0.810556943750001,30.7145833342893,1.40392580900275));
#5347=CARTESIAN_POINT('Ctrl Pts',(3.43862649647115E-16,30.6562500009559,
1.87190107867033));
#5348=CARTESIAN_POINT('Ctrl Pts',(-0.810556943749999,30.5979166676226,1.40392580900275));
#5349=CARTESIAN_POINT('Ctrl Pts',(-1.6211138875,30.5395833342893,0.935950539335167));
#5350=CARTESIAN_POINT('Ctrl Pts',(-1.6211138875,30.4812500009559,0.));
#5351=CARTESIAN_POINT('Ctrl Pts',(-1.6211138875,30.4229166676226,-0.935950539335166));
#5352=CARTESIAN_POINT('Ctrl Pts',(-0.81055694375,30.3645833342893,-1.40392580900275));
#5353=CARTESIAN_POINT('Ctrl Pts',(-1.14620883215705E-16,30.3062500009559,
-1.87190107867033));
#5354=CARTESIAN_POINT('Ctrl Pts',(0.81055694375,30.2479166676226,-1.40392580900275));
#5355=CARTESIAN_POINT('Ctrl Pts',(1.6211138875,30.1895833342893,-0.935950539335166));
#5356=CARTESIAN_POINT('Ctrl Pts',(1.6211138875,30.1312500009559,-1.9852919333802E-16));
#5357=CARTESIAN_POINT('Ctrl Pts',(1.6211138875,30.0729166676226,0.935950539335165));
#5358=CARTESIAN_POINT('Ctrl Pts',(0.810556943750001,30.0145833342893,1.40392580900275));
#5359=CARTESIAN_POINT('Ctrl Pts',(3.43862649647115E-16,29.9562500009559,
1.87190107867033));
#5360=CARTESIAN_POINT('Ctrl Pts',(-0.810556943749999,29.8979166676226,1.40392580900275));
#5361=CARTESIAN_POINT('Ctrl Pts',(-1.6211138875,29.8395833342892,0.935950539335167));
#5362=CARTESIAN_POINT('Ctrl Pts',(-1.6211138875,29.7812500009559,0.));
#5363=CARTESIAN_POINT('Ctrl Pts',(-1.6211138875,29.7229166676226,-0.935950539335166));
#5364=CARTESIAN_POINT('Ctrl Pts',(-0.81055694375,29.6645833342893,-1.40392580900275));
#5365=CARTESIAN_POINT('Ctrl Pts',(-1.14620883215705E-16,29.6062500009559,
-1.87190107867033));
#5366=CARTESIAN_POINT('Ctrl Pts',(0.81055694375,29.5479166676226,-1.40392580900275));
#5367=CARTESIAN_POINT('Ctrl Pts',(1.6211138875,29.4895833342893,-0.935950539335166));
#5368=CARTESIAN_POINT('Ctrl Pts',(1.6211138875,29.4312500009559,-1.9852919333802E-16));
#5369=CARTESIAN_POINT('Ctrl Pts',(1.6211138875,29.3729166676226,0.935950539335165));
#5370=CARTESIAN_POINT('Ctrl Pts',(0.810556943750001,29.3145833342893,1.40392580900275));
#5371=CARTESIAN_POINT('Ctrl Pts',(3.43862649647115E-16,29.2562500009559,
1.87190107867033));
#5372=CARTESIAN_POINT('Ctrl Pts',(-0.810556943749999,29.1979166676226,1.40392580900275));
#5373=CARTESIAN_POINT('Ctrl Pts',(-1.6211138875,29.1395833342893,0.935950539335167));
#5374=CARTESIAN_POINT('Ctrl Pts',(-1.6211138875,29.0812500009559,0.));
#5375=CARTESIAN_POINT('Ctrl Pts',(-1.6211138875,29.0229166676226,-0.935950539335166));
#5376=CARTESIAN_POINT('Ctrl Pts',(-0.81055694375,28.9645833342893,-1.40392580900275));
#5377=CARTESIAN_POINT('Ctrl Pts',(-1.14620883215705E-16,28.9062500009559,
-1.87190107867033));
#5378=CARTESIAN_POINT('Ctrl Pts',(0.81055694375,28.8479166676226,-1.40392580900275));
#5379=CARTESIAN_POINT('Ctrl Pts',(1.6211138875,28.7895833342893,-0.935950539335166));
#5380=CARTESIAN_POINT('Ctrl Pts',(1.6211138875,28.7312500009559,-1.9852919333802E-16));
#5381=CARTESIAN_POINT('Ctrl Pts',(1.6211138875,28.6729166676226,0.935950539335165));
#5382=CARTESIAN_POINT('Ctrl Pts',(0.810556943750001,28.6145833342893,1.40392580900275));
#5383=CARTESIAN_POINT('Ctrl Pts',(3.43862649647115E-16,28.5562500009559,
1.87190107867033));
#5384=CARTESIAN_POINT('Ctrl Pts',(-0.810556943749999,28.4979166676226,1.40392580900275));
#5385=CARTESIAN_POINT('Ctrl Pts',(-1.6211138875,28.4395833342893,0.935950539335167));
#5386=CARTESIAN_POINT('Ctrl Pts',(-1.6211138875,28.3812500009559,0.));
#5387=CARTESIAN_POINT('Ctrl Pts',(-1.6211138875,28.3229166676226,-0.935950539335166));
#5388=CARTESIAN_POINT('Ctrl Pts',(-0.81055694375,28.2645833342893,-1.40392580900275));
#5389=CARTESIAN_POINT('Ctrl Pts',(-1.14620883215705E-16,28.2062500009559,
-1.87190107867033));
#5390=CARTESIAN_POINT('Ctrl Pts',(0.81055694375,28.1479166676226,-1.40392580900275));
#5391=CARTESIAN_POINT('Ctrl Pts',(1.6211138875,28.0895833342893,-0.935950539335166));
#5392=CARTESIAN_POINT('Ctrl Pts',(1.6211138875,28.0312500009559,-1.9852919333802E-16));
#5393=CARTESIAN_POINT('Ctrl Pts',(1.6211138875,27.9729166676226,0.935950539335165));
#5394=CARTESIAN_POINT('Ctrl Pts',(0.810556943750001,27.9145833342893,1.40392580900275));
#5395=CARTESIAN_POINT('Ctrl Pts',(3.43862649647115E-16,27.8562500009559,
1.87190107867033));
#5396=CARTESIAN_POINT('Ctrl Pts',(-0.810556943749999,27.7979166676226,1.40392580900275));
#5397=CARTESIAN_POINT('Ctrl Pts',(-1.6211138875,27.7395833342893,0.935950539335167));
#5398=CARTESIAN_POINT('Ctrl Pts',(-1.6211138875,27.6812500009559,0.));
#5399=CARTESIAN_POINT('Ctrl Pts',(-1.6211138875,27.6229166676226,-0.935950539335166));
#5400=CARTESIAN_POINT('Ctrl Pts',(-0.81055694375,27.5645833342893,-1.40392580900275));
#5401=CARTESIAN_POINT('Ctrl Pts',(-1.14620883215705E-16,27.5062500009559,
-1.87190107867033));
#5402=CARTESIAN_POINT('Ctrl Pts',(0.81055694375,27.4479166676226,-1.40392580900275));
#5403=CARTESIAN_POINT('Ctrl Pts',(1.6211138875,27.3895833342893,-0.935950539335166));
#5404=CARTESIAN_POINT('Ctrl Pts',(1.6211138875,27.3312500009559,-1.9852919333802E-16));
#5405=CARTESIAN_POINT('Ctrl Pts',(1.6211138875,27.2729166676226,0.935950539335165));
#5406=CARTESIAN_POINT('Ctrl Pts',(0.810556943750001,27.2145833342893,1.40392580900275));
#5407=CARTESIAN_POINT('Ctrl Pts',(3.43862649647115E-16,27.1562500009559,
1.87190107867033));
#5408=CARTESIAN_POINT('Ctrl Pts',(-0.810556943749999,27.0979166676226,1.40392580900275));
#5409=CARTESIAN_POINT('Ctrl Pts',(-1.6211138875,27.0395833342893,0.935950539335167));
#5410=CARTESIAN_POINT('Ctrl Pts',(-1.6211138875,26.9812500009559,0.));
#5411=CARTESIAN_POINT('Ctrl Pts',(-1.6211138875,26.9229166676226,-0.935950539335166));
#5412=CARTESIAN_POINT('Ctrl Pts',(-0.81055694375,26.8645833342893,-1.40392580900275));
#5413=CARTESIAN_POINT('Ctrl Pts',(-1.14620883215705E-16,26.8062500009559,
-1.87190107867033));
#5414=CARTESIAN_POINT('Ctrl Pts',(0.81055694375,26.7479166676226,-1.40392580900275));
#5415=CARTESIAN_POINT('Ctrl Pts',(1.6211138875,26.6895833342893,-0.935950539335166));
#5416=CARTESIAN_POINT('Ctrl Pts',(1.6211138875,26.6312500009559,-1.9852919333802E-16));
#5417=CARTESIAN_POINT('Ctrl Pts',(1.6211138875,26.5729166676226,0.935950539335165));
#5418=CARTESIAN_POINT('Ctrl Pts',(0.810556943750001,26.5145833342893,1.40392580900275));
#5419=CARTESIAN_POINT('Ctrl Pts',(3.43862649647115E-16,26.4562500009559,
1.87190107867033));
#5420=CARTESIAN_POINT('Ctrl Pts',(-0.810556943749999,26.3979166676226,1.40392580900275));
#5421=CARTESIAN_POINT('Ctrl Pts',(-1.6211138875,26.3395833342893,0.935950539335167));
#5422=CARTESIAN_POINT('Ctrl Pts',(-1.6211138875,26.2812500009559,0.));
#5423=CARTESIAN_POINT('Ctrl Pts',(-1.6211138875,26.2229166676226,-0.935950539335166));
#5424=CARTESIAN_POINT('Ctrl Pts',(-0.81055694375,26.1645833342893,-1.40392580900275));
#5425=CARTESIAN_POINT('Ctrl Pts',(-1.14620883215705E-16,26.1062500009559,
-1.87190107867033));
#5426=CARTESIAN_POINT('Ctrl Pts',(0.81055694375,26.0479166676226,-1.40392580900275));
#5427=CARTESIAN_POINT('Ctrl Pts',(1.6211138875,25.9895833342893,-0.935950539335166));
#5428=CARTESIAN_POINT('Ctrl Pts',(1.6211138875,25.9312500009559,-1.9852919333802E-16));
#5429=CARTESIAN_POINT('Ctrl Pts',(1.6211138875,25.8729166676226,0.935950539335165));
#5430=CARTESIAN_POINT('Ctrl Pts',(0.810556943750001,25.8145833342892,1.40392580900275));
#5431=CARTESIAN_POINT('Ctrl Pts',(3.43862649647115E-16,25.7562500009559,
1.87190107867033));
#5432=CARTESIAN_POINT('Ctrl Pts',(-0.810556943749999,25.6979166676226,1.40392580900275));
#5433=CARTESIAN_POINT('Ctrl Pts',(-1.6211138875,25.6395833342893,0.935950539335167));
#5434=CARTESIAN_POINT('Ctrl Pts',(-1.6211138875,25.5812500009559,0.));
#5435=CARTESIAN_POINT('Ctrl Pts',(-1.6211138875,25.5229166676226,-0.935950539335166));
#5436=CARTESIAN_POINT('Ctrl Pts',(-0.81055694375,25.4645833342893,-1.40392580900275));
#5437=CARTESIAN_POINT('Ctrl Pts',(-1.14620883215705E-16,25.4062500009559,
-1.87190107867033));
#5438=CARTESIAN_POINT('Ctrl Pts',(0.81055694375,25.3479166676226,-1.40392580900275));
#5439=CARTESIAN_POINT('Ctrl Pts',(1.6211138875,25.2895833342893,-0.935950539335166));
#5440=CARTESIAN_POINT('Ctrl Pts',(1.6211138875,25.2312500009559,-1.9852919333802E-16));
#5441=CARTESIAN_POINT('Ctrl Pts',(1.6211138875,25.1729166676226,0.935950539335165));
#5442=CARTESIAN_POINT('Ctrl Pts',(0.810556943750001,25.1145833342893,1.40392580900275));
#5443=CARTESIAN_POINT('Ctrl Pts',(3.43862649647115E-16,25.0562500009559,
1.87190107867033));
#5444=CARTESIAN_POINT('Ctrl Pts',(-0.810556943749999,24.9979166676226,1.40392580900275));
#5445=CARTESIAN_POINT('Ctrl Pts',(-1.6211138875,24.9395833342893,0.935950539335167));
#5446=CARTESIAN_POINT('Ctrl Pts',(-1.6211138875,24.8812500009559,0.));
#5447=CARTESIAN_POINT('Ctrl Pts',(-1.6211138875,24.8229166676226,-0.935950539335166));
#5448=CARTESIAN_POINT('Ctrl Pts',(-0.81055694375,24.7645833342893,-1.40392580900275));
#5449=CARTESIAN_POINT('Ctrl Pts',(-1.14620883215705E-16,24.7062500009559,
-1.87190107867033));
#5450=CARTESIAN_POINT('Ctrl Pts',(0.81055694375,24.6479166676226,-1.40392580900275));
#5451=CARTESIAN_POINT('Ctrl Pts',(1.6211138875,24.5895833342893,-0.935950539335166));
#5452=CARTESIAN_POINT('Ctrl Pts',(1.6211138875,24.5312500009559,-1.9852919333802E-16));
#5453=CARTESIAN_POINT('Ctrl Pts',(1.6211138875,24.4729166676226,0.935950539335165));
#5454=CARTESIAN_POINT('Ctrl Pts',(0.810556943750001,24.4145833342893,1.40392580900275));
#5455=CARTESIAN_POINT('Ctrl Pts',(3.43862649647115E-16,24.3562500009559,
1.87190107867033));
#5456=CARTESIAN_POINT('Ctrl Pts',(-0.810556943749999,24.2979166676226,1.40392580900275));
#5457=CARTESIAN_POINT('Ctrl Pts',(-1.6211138875,24.2395833342893,0.935950539335167));
#5458=CARTESIAN_POINT('Ctrl Pts',(-1.6211138875,24.1812500009559,0.));
#5459=CARTESIAN_POINT('Ctrl Pts',(-1.6211138875,24.1229166676226,-0.935950539335166));
#5460=CARTESIAN_POINT('Ctrl Pts',(-0.81055694375,24.0645833342893,-1.40392580900275));
#5461=CARTESIAN_POINT('Ctrl Pts',(-1.14620883215705E-16,24.0062500009559,
-1.87190107867033));
#5462=CARTESIAN_POINT('Ctrl Pts',(0.81055694375,23.9479166676226,-1.40392580900275));
#5463=CARTESIAN_POINT('Ctrl Pts',(1.6211138875,23.8895833342893,-0.935950539335166));
#5464=CARTESIAN_POINT('Ctrl Pts',(1.6211138875,23.8312500009559,-1.9852919333802E-16));
#5465=CARTESIAN_POINT('Ctrl Pts',(1.6211138875,23.7729166676226,0.935950539335165));
#5466=CARTESIAN_POINT('Ctrl Pts',(0.810556943750001,23.7145833342893,1.40392580900275));
#5467=CARTESIAN_POINT('Ctrl Pts',(3.43862649647115E-16,23.6562500009559,
1.87190107867033));
#5468=CARTESIAN_POINT('Ctrl Pts',(-0.810556943749999,23.5979166676226,1.40392580900275));
#5469=CARTESIAN_POINT('Ctrl Pts',(-1.6211138875,23.5395833342893,0.935950539335167));
#5470=CARTESIAN_POINT('Ctrl Pts',(-1.6211138875,23.4812500009559,0.));
#5471=CARTESIAN_POINT('Ctrl Pts',(-1.6211138875,23.4229166676226,-0.935950539335166));
#5472=CARTESIAN_POINT('Ctrl Pts',(-0.81055694375,23.3645833342893,-1.40392580900275));
#5473=CARTESIAN_POINT('Ctrl Pts',(-1.14620883215705E-16,23.3062500009559,
-1.87190107867033));
#5474=CARTESIAN_POINT('Ctrl Pts',(0.81055694375,23.2479166676226,-1.40392580900275));
#5475=CARTESIAN_POINT('Ctrl Pts',(1.6211138875,23.1895833342893,-0.935950539335166));
#5476=CARTESIAN_POINT('Ctrl Pts',(1.6211138875,23.1312500009559,-1.9852919333802E-16));
#5477=CARTESIAN_POINT('Ctrl Pts',(1.6211138875,23.0729166676226,0.935950539335165));
#5478=CARTESIAN_POINT('Ctrl Pts',(0.810556943750001,23.0145833342893,1.40392580900275));
#5479=CARTESIAN_POINT('Ctrl Pts',(3.43862649647115E-16,22.9562500009559,
1.87190107867033));
#5480=CARTESIAN_POINT('Ctrl Pts',(-0.810556943749999,22.8979166676226,1.40392580900275));
#5481=CARTESIAN_POINT('Ctrl Pts',(-1.6211138875,22.8395833342893,0.935950539335167));
#5482=CARTESIAN_POINT('Ctrl Pts',(-1.6211138875,22.7812500009559,0.));
#5483=CARTESIAN_POINT('Ctrl Pts',(-1.6211138875,22.7229166676226,-0.935950539335166));
#5484=CARTESIAN_POINT('Ctrl Pts',(-0.81055694375,22.6645833342893,-1.40392580900275));
#5485=CARTESIAN_POINT('Ctrl Pts',(-1.14620883215705E-16,22.6062500009559,
-1.87190107867033));
#5486=CARTESIAN_POINT('Ctrl Pts',(0.81055694375,22.5479166676226,-1.40392580900275));
#5487=CARTESIAN_POINT('Ctrl Pts',(1.6211138875,22.4895833342893,-0.935950539335166));
#5488=CARTESIAN_POINT('Ctrl Pts',(1.6211138875,22.4312500009559,-1.9852919333802E-16));
#5489=CARTESIAN_POINT('Ctrl Pts',(1.6211138875,22.3729166676226,0.935950539335165));
#5490=CARTESIAN_POINT('Ctrl Pts',(0.810556943750001,22.3145833342893,1.40392580900275));
#5491=CARTESIAN_POINT('Ctrl Pts',(3.43862649647115E-16,22.2562500009559,
1.87190107867033));
#5492=CARTESIAN_POINT('Ctrl Pts',(-0.810556943749999,22.1979166676226,1.40392580900275));
#5493=CARTESIAN_POINT('Ctrl Pts',(-1.6211138875,22.1395833342893,0.935950539335167));
#5494=CARTESIAN_POINT('Ctrl Pts',(-1.6211138875,22.0812500009559,0.));
#5495=CARTESIAN_POINT('Ctrl Pts',(-1.6211138875,22.0229166676226,-0.935950539335166));
#5496=CARTESIAN_POINT('Ctrl Pts',(-0.81055694375,21.9645833342893,-1.40392580900275));
#5497=CARTESIAN_POINT('Ctrl Pts',(-1.14620883215705E-16,21.9062500009559,
-1.87190107867033));
#5498=CARTESIAN_POINT('Ctrl Pts',(0.81055694375,21.8479166676226,-1.40392580900275));
#5499=CARTESIAN_POINT('Ctrl Pts',(1.6211138875,21.7895833342893,-0.935950539335166));
#5500=CARTESIAN_POINT('Ctrl Pts',(1.6211138875,21.7312500009559,-1.9852919333802E-16));
#5501=CARTESIAN_POINT('Ctrl Pts',(1.6211138875,21.6729166676226,0.935950539335165));
#5502=CARTESIAN_POINT('Ctrl Pts',(0.810556943750001,21.6145833342893,1.40392580900275));
#5503=CARTESIAN_POINT('Ctrl Pts',(3.43862649647115E-16,21.5562500009559,
1.87190107867033));
#5504=CARTESIAN_POINT('Ctrl Pts',(-0.810556943749999,21.4979166676226,1.40392580900275));
#5505=CARTESIAN_POINT('Ctrl Pts',(-1.6211138875,21.4395833342893,0.935950539335167));
#5506=CARTESIAN_POINT('Ctrl Pts',(-1.6211138875,21.3812500009559,0.));
#5507=CARTESIAN_POINT('Ctrl Pts',(-1.6211138875,21.3229166676226,-0.935950539335166));
#5508=CARTESIAN_POINT('Ctrl Pts',(-0.81055694375,21.2645833342893,-1.40392580900275));
#5509=CARTESIAN_POINT('Ctrl Pts',(-1.14620883215705E-16,21.2062500009559,
-1.87190107867033));
#5510=CARTESIAN_POINT('Ctrl Pts',(0.81055694375,21.1479166676226,-1.40392580900275));
#5511=CARTESIAN_POINT('Ctrl Pts',(1.6211138875,21.0895833342892,-0.935950539335166));
#5512=CARTESIAN_POINT('Ctrl Pts',(1.6211138875,21.0312500009559,-1.9852919333802E-16));
#5513=CARTESIAN_POINT('Ctrl Pts',(1.6211138875,20.9729166676226,0.935950539335165));
#5514=CARTESIAN_POINT('Ctrl Pts',(0.810556943750001,20.9145833342893,1.40392580900275));
#5515=CARTESIAN_POINT('Ctrl Pts',(3.43862649647115E-16,20.8562500009559,
1.87190107867033));
#5516=CARTESIAN_POINT('Ctrl Pts',(-0.810556943749999,20.7979166676226,1.40392580900275));
#5517=CARTESIAN_POINT('Ctrl Pts',(-1.6211138875,20.7395833342893,0.935950539335167));
#5518=CARTESIAN_POINT('Ctrl Pts',(-1.6211138875,20.6812500009559,0.));
#5519=CARTESIAN_POINT('Ctrl Pts',(-1.6211138875,20.6229166676226,-0.935950539335166));
#5520=CARTESIAN_POINT('Ctrl Pts',(-0.81055694375,20.5645833342893,-1.40392580900275));
#5521=CARTESIAN_POINT('Ctrl Pts',(-1.14620883215705E-16,20.5062500009559,
-1.87190107867033));
#5522=CARTESIAN_POINT('Ctrl Pts',(0.81055694375,20.4479166676226,-1.40392580900275));
#5523=CARTESIAN_POINT('Ctrl Pts',(1.6211138875,20.3895833342893,-0.935950539335166));
#5524=CARTESIAN_POINT('Ctrl Pts',(1.6211138875,20.3312500009559,-1.9852919333802E-16));
#5525=CARTESIAN_POINT('Ctrl Pts',(1.6211138875,20.2729166676226,0.935950539335165));
#5526=CARTESIAN_POINT('Ctrl Pts',(0.810556943750001,20.2145833342893,1.40392580900275));
#5527=CARTESIAN_POINT('Ctrl Pts',(3.43862649647115E-16,20.1562500009559,
1.87190107867033));
#5528=CARTESIAN_POINT('Ctrl Pts',(-0.810556943749999,20.0979166676226,1.40392580900275));
#5529=CARTESIAN_POINT('Ctrl Pts',(-1.6211138875,20.0395833342893,0.935950539335167));
#5530=CARTESIAN_POINT('Ctrl Pts',(-1.6211138875,19.9812500009559,0.));
#5531=CARTESIAN_POINT('Ctrl Pts',(-1.6211138875,19.9229166676226,-0.935950539335166));
#5532=CARTESIAN_POINT('Ctrl Pts',(-0.81055694375,19.8645833342893,-1.40392580900275));
#5533=CARTESIAN_POINT('Ctrl Pts',(-1.14620883215705E-16,19.8062500009559,
-1.87190107867033));
#5534=CARTESIAN_POINT('Ctrl Pts',(0.81055694375,19.7479166676226,-1.40392580900275));
#5535=CARTESIAN_POINT('Ctrl Pts',(1.6211138875,19.6895833342893,-0.935950539335166));
#5536=CARTESIAN_POINT('Ctrl Pts',(1.6211138875,19.6312500009559,-1.9852919333802E-16));
#5537=CARTESIAN_POINT('Ctrl Pts',(1.6211138875,19.5729166676226,0.935950539335165));
#5538=CARTESIAN_POINT('Ctrl Pts',(0.810556943750001,19.5145833342893,1.40392580900275));
#5539=CARTESIAN_POINT('Ctrl Pts',(3.43862649647115E-16,19.4562500009559,
1.87190107867033));
#5540=CARTESIAN_POINT('Ctrl Pts',(-0.810556943749999,19.3979166676226,1.40392580900275));
#5541=CARTESIAN_POINT('Ctrl Pts',(-1.6211138875,19.3395833342893,0.935950539335167));
#5542=CARTESIAN_POINT('Ctrl Pts',(-1.6211138875,19.2812500009559,0.));
#5543=CARTESIAN_POINT('Ctrl Pts',(-1.6211138875,19.2229166676226,-0.935950539335166));
#5544=CARTESIAN_POINT('Ctrl Pts',(-0.81055694375,19.1645833342893,-1.40392580900275));
#5545=CARTESIAN_POINT('Ctrl Pts',(-1.14620883215705E-16,19.1062500009559,
-1.87190107867033));
#5546=CARTESIAN_POINT('Ctrl Pts',(0.81055694375,19.0479166676226,-1.40392580900275));
#5547=CARTESIAN_POINT('Ctrl Pts',(1.6211138875,18.9895833342893,-0.935950539335166));
#5548=CARTESIAN_POINT('Ctrl Pts',(1.6211138875,18.9312500009559,-1.9852919333802E-16));
#5549=CARTESIAN_POINT('Ctrl Pts',(1.6211138875,18.8729166676226,0.935950539335165));
#5550=CARTESIAN_POINT('Ctrl Pts',(0.810556943750001,18.8145833342893,1.40392580900275));
#5551=CARTESIAN_POINT('Ctrl Pts',(3.43862649647115E-16,18.7562500009559,
1.87190107867033));
#5552=CARTESIAN_POINT('Ctrl Pts',(-0.810556943749999,18.6979166676226,1.40392580900275));
#5553=CARTESIAN_POINT('Ctrl Pts',(-1.6211138875,18.6395833342893,0.935950539335167));
#5554=CARTESIAN_POINT('Ctrl Pts',(-1.6211138875,18.5812500009559,0.));
#5555=CARTESIAN_POINT('Ctrl Pts',(-1.6211138875,18.5229166676226,-0.935950539335166));
#5556=CARTESIAN_POINT('Ctrl Pts',(-0.81055694375,18.4645833342893,-1.40392580900275));
#5557=CARTESIAN_POINT('Ctrl Pts',(-1.14620883215705E-16,18.4062500009559,
-1.87190107867033));
#5558=CARTESIAN_POINT('Ctrl Pts',(0.81055694375,18.3479166676226,-1.40392580900275));
#5559=CARTESIAN_POINT('Ctrl Pts',(1.6211138875,18.2895833342893,-0.935950539335166));
#5560=CARTESIAN_POINT('Ctrl Pts',(1.6211138875,18.2312500009559,-1.9852919333802E-16));
#5561=CARTESIAN_POINT('Ctrl Pts',(1.6211138875,18.1729166676226,0.935950539335165));
#5562=CARTESIAN_POINT('Ctrl Pts',(0.810556943750001,18.1145833342893,1.40392580900275));
#5563=CARTESIAN_POINT('Ctrl Pts',(3.43862649647115E-16,18.0562500009559,
1.87190107867033));
#5564=CARTESIAN_POINT('Ctrl Pts',(-0.810556943749999,17.9979166676226,1.40392580900275));
#5565=CARTESIAN_POINT('Ctrl Pts',(-1.6211138875,17.9395833342893,0.935950539335167));
#5566=CARTESIAN_POINT('Ctrl Pts',(-1.6211138875,17.8812500009559,0.));
#5567=CARTESIAN_POINT('Ctrl Pts',(-1.6211138875,17.8229166676226,-0.935950539335166));
#5568=CARTESIAN_POINT('Ctrl Pts',(-0.81055694375,17.7645833342893,-1.40392580900275));
#5569=CARTESIAN_POINT('Ctrl Pts',(-1.14620883215705E-16,17.7062500009559,
-1.87190107867033));
#5570=CARTESIAN_POINT('Ctrl Pts',(0.81055694375,17.6479166676226,-1.40392580900275));
#5571=CARTESIAN_POINT('Ctrl Pts',(1.6211138875,17.5895833342893,-0.935950539335166));
#5572=CARTESIAN_POINT('Ctrl Pts',(1.6211138875,17.5312500009559,-1.9852919333802E-16));
#5573=CARTESIAN_POINT('Ctrl Pts',(1.6211138875,17.4729166676226,0.935950539335165));
#5574=CARTESIAN_POINT('Ctrl Pts',(0.810556943750001,17.4145833342893,1.40392580900275));
#5575=CARTESIAN_POINT('Ctrl Pts',(3.43862649647115E-16,17.3562500009559,
1.87190107867033));
#5576=CARTESIAN_POINT('Ctrl Pts',(-0.810556943749999,17.2979166676226,1.40392580900275));
#5577=CARTESIAN_POINT('Ctrl Pts',(-1.6211138875,17.2395833342893,0.935950539335167));
#5578=CARTESIAN_POINT('Ctrl Pts',(-1.6211138875,17.1812500009559,0.));
#5579=CARTESIAN_POINT('Ctrl Pts',(-1.6211138875,17.1229166676226,-0.935950539335166));
#5580=CARTESIAN_POINT('Ctrl Pts',(-0.81055694375,17.0645833342893,-1.40392580900275));
#5581=CARTESIAN_POINT('Ctrl Pts',(-1.14620883215705E-16,17.0062500009559,
-1.87190107867033));
#5582=CARTESIAN_POINT('Ctrl Pts',(0.81055694375,16.9479166676226,-1.40392580900275));
#5583=CARTESIAN_POINT('Ctrl Pts',(1.6211138875,16.8895833342893,-0.935950539335166));
#5584=CARTESIAN_POINT('Ctrl Pts',(1.6211138875,16.8312500009559,-1.9852919333802E-16));
#5585=CARTESIAN_POINT('Ctrl Pts',(1.6211138875,16.7729166676226,0.935950539335165));
#5586=CARTESIAN_POINT('Ctrl Pts',(0.810556943750001,16.7145833342893,1.40392580900275));
#5587=CARTESIAN_POINT('Ctrl Pts',(3.43862649647115E-16,16.6562500009559,
1.87190107867033));
#5588=CARTESIAN_POINT('Ctrl Pts',(-0.810556943749999,16.5979166676226,1.40392580900275));
#5589=CARTESIAN_POINT('Ctrl Pts',(-1.6211138875,16.5395833342893,0.935950539335167));
#5590=CARTESIAN_POINT('Ctrl Pts',(-1.6211138875,16.4812500009559,0.));
#5591=CARTESIAN_POINT('Ctrl Pts',(-1.6211138875,16.4229166676226,-0.935950539335166));
#5592=CARTESIAN_POINT('Ctrl Pts',(-0.81055694375,16.3645833342893,-1.40392580900275));
#5593=CARTESIAN_POINT('Ctrl Pts',(-1.14620883215705E-16,16.3062500009559,
-1.87190107867033));
#5594=CARTESIAN_POINT('Ctrl Pts',(0.81055694375,16.2479166676226,-1.40392580900275));
#5595=CARTESIAN_POINT('Ctrl Pts',(1.6211138875,16.1895833342893,-0.935950539335166));
#5596=CARTESIAN_POINT('Ctrl Pts',(1.6211138875,16.1312500009559,-1.9852919333802E-16));
#5597=CARTESIAN_POINT('Ctrl Pts',(1.6211138875,16.0729166676226,0.935950539335165));
#5598=CARTESIAN_POINT('Ctrl Pts',(0.810556943750001,16.0145833342893,1.40392580900275));
#5599=CARTESIAN_POINT('Ctrl Pts',(3.43862649647115E-16,15.9562500009559,
1.87190107867033));
#5600=CARTESIAN_POINT('Ctrl Pts',(-0.810556943749999,15.8979166676226,1.40392580900275));
#5601=CARTESIAN_POINT('Ctrl Pts',(-1.6211138875,15.8395833342893,0.935950539335167));
#5602=CARTESIAN_POINT('Ctrl Pts',(-1.6211138875,15.7812500009559,0.));
#5603=CARTESIAN_POINT('Ctrl Pts',(-1.6211138875,15.7229166676226,-0.935950539335166));
#5604=CARTESIAN_POINT('Ctrl Pts',(-0.81055694375,15.6645833342893,-1.40392580900275));
#5605=CARTESIAN_POINT('Ctrl Pts',(-1.14620883215705E-16,15.6062500009559,
-1.87190107867033));
#5606=CARTESIAN_POINT('Ctrl Pts',(0.81055694375,15.5479166676226,-1.40392580900275));
#5607=CARTESIAN_POINT('Ctrl Pts',(1.6211138875,15.4895833342893,-0.935950539335166));
#5608=CARTESIAN_POINT('Ctrl Pts',(1.6211138875,15.4312500009559,-1.9852919333802E-16));
#5609=CARTESIAN_POINT('Ctrl Pts',(1.6211138875,15.3729166676226,0.935950539335165));
#5610=CARTESIAN_POINT('Ctrl Pts',(0.810556943750001,15.3145833342893,1.40392580900275));
#5611=CARTESIAN_POINT('Ctrl Pts',(3.43862649647115E-16,15.2562500009559,
1.87190107867033));
#5612=CARTESIAN_POINT('Ctrl Pts',(-0.810556943749999,15.1979166676226,1.40392580900275));
#5613=CARTESIAN_POINT('Ctrl Pts',(-1.6211138875,15.1395833342893,0.935950539335167));
#5614=CARTESIAN_POINT('Ctrl Pts',(-1.6211138875,15.0812500009559,0.));
#5615=CARTESIAN_POINT('Ctrl Pts',(-1.6211138875,15.0229166676226,-0.935950539335166));
#5616=CARTESIAN_POINT('Ctrl Pts',(-0.81055694375,14.9645833342893,-1.40392580900275));
#5617=CARTESIAN_POINT('Ctrl Pts',(-1.14620883215705E-16,14.9062500009559,
-1.87190107867033));
#5618=CARTESIAN_POINT('Ctrl Pts',(0.81055694375,14.8479166676226,-1.40392580900275));
#5619=CARTESIAN_POINT('Ctrl Pts',(1.6211138875,14.7895833342893,-0.935950539335166));
#5620=CARTESIAN_POINT('Ctrl Pts',(1.6211138875,14.7312500009559,-1.9852919333802E-16));
#5621=CARTESIAN_POINT('Ctrl Pts',(1.6211138875,14.6729166676226,0.935950539335165));
#5622=CARTESIAN_POINT('Ctrl Pts',(0.810556943750001,14.6145833342893,1.40392580900275));
#5623=CARTESIAN_POINT('Ctrl Pts',(3.43862649647115E-16,14.5562500009559,
1.87190107867033));
#5624=CARTESIAN_POINT('Ctrl Pts',(-0.810556943749999,14.4979166676226,1.40392580900275));
#5625=CARTESIAN_POINT('Ctrl Pts',(-1.6211138875,14.4395833342893,0.935950539335167));
#5626=CARTESIAN_POINT('Ctrl Pts',(-1.6211138875,14.3812500009559,0.));
#5627=CARTESIAN_POINT('Ctrl Pts',(-1.6211138875,14.3229166676226,-0.935950539335166));
#5628=CARTESIAN_POINT('Ctrl Pts',(-0.81055694375,14.2645833342893,-1.40392580900275));
#5629=CARTESIAN_POINT('Ctrl Pts',(-1.14620883215705E-16,14.2062500009559,
-1.87190107867033));
#5630=CARTESIAN_POINT('Ctrl Pts',(0.81055694375,14.1479166676226,-1.40392580900275));
#5631=CARTESIAN_POINT('Ctrl Pts',(1.6211138875,14.0895833342893,-0.935950539335166));
#5632=CARTESIAN_POINT('Ctrl Pts',(1.6211138875,14.0312500009559,-1.9852919333802E-16));
#5633=CARTESIAN_POINT('Ctrl Pts',(1.6211138875,13.9729166676226,0.935950539335165));
#5634=CARTESIAN_POINT('Ctrl Pts',(0.810556943750001,13.9145833342893,1.40392580900275));
#5635=CARTESIAN_POINT('Ctrl Pts',(3.43862649647115E-16,13.8562500009559,
1.87190107867033));
#5636=CARTESIAN_POINT('Ctrl Pts',(-0.810556943749999,13.7979166676226,1.40392580900275));
#5637=CARTESIAN_POINT('Ctrl Pts',(-1.6211138875,13.7395833342893,0.935950539335167));
#5638=CARTESIAN_POINT('Ctrl Pts',(-1.6211138875,13.6812500009559,0.));
#5639=CARTESIAN_POINT('Ctrl Pts',(-1.6211138875,13.6229166676226,-0.935950539335166));
#5640=CARTESIAN_POINT('Ctrl Pts',(-0.81055694375,13.5645833342893,-1.40392580900275));
#5641=CARTESIAN_POINT('Ctrl Pts',(-1.14620883215705E-16,13.5062500009559,
-1.87190107867033));
#5642=CARTESIAN_POINT('Ctrl Pts',(0.81055694375,13.4479166676226,-1.40392580900275));
#5643=CARTESIAN_POINT('Ctrl Pts',(1.6211138875,13.3895833342893,-0.935950539335166));
#5644=CARTESIAN_POINT('Ctrl Pts',(1.6211138875,13.3312500009559,-1.9852919333802E-16));
#5645=CARTESIAN_POINT('Ctrl Pts',(1.6211138875,13.2729166676226,0.935950539335165));
#5646=CARTESIAN_POINT('Ctrl Pts',(0.810556943750001,13.2145833342893,1.40392580900275));
#5647=CARTESIAN_POINT('Ctrl Pts',(3.43862649647115E-16,13.1562500009559,
1.87190107867033));
#5648=CARTESIAN_POINT('Ctrl Pts',(-0.810556943749999,13.0979166676226,1.40392580900275));
#5649=CARTESIAN_POINT('Ctrl Pts',(-1.6211138875,13.0395833342893,0.935950539335167));
#5650=CARTESIAN_POINT('Ctrl Pts',(-1.6211138875,12.9812500009559,0.));
#5651=CARTESIAN_POINT('Ctrl Pts',(-1.6211138875,12.9229166676226,-0.935950539335166));
#5652=CARTESIAN_POINT('Ctrl Pts',(-0.81055694375,12.8645833342893,-1.40392580900275));
#5653=CARTESIAN_POINT('Ctrl Pts',(-1.14620883215705E-16,12.8062500009559,
-1.87190107867033));
#5654=CARTESIAN_POINT('Ctrl Pts',(0.81055694375,12.7479166676226,-1.40392580900275));
#5655=CARTESIAN_POINT('Ctrl Pts',(1.6211138875,12.6895833342893,-0.935950539335166));
#5656=CARTESIAN_POINT('Ctrl Pts',(1.6211138875,12.6312500009559,-1.9852919333802E-16));
#5657=CARTESIAN_POINT('Ctrl Pts',(1.6211138875,12.5729166676226,0.935950539335165));
#5658=CARTESIAN_POINT('Ctrl Pts',(0.810556943750001,12.5145833342893,1.40392580900275));
#5659=CARTESIAN_POINT('Ctrl Pts',(3.43862649647115E-16,12.4562500009559,
1.87190107867033));
#5660=CARTESIAN_POINT('Ctrl Pts',(-0.810556943749999,12.3979166676226,1.40392580900275));
#5661=CARTESIAN_POINT('Ctrl Pts',(-1.6211138875,12.3395833342893,0.935950539335167));
#5662=CARTESIAN_POINT('Ctrl Pts',(-1.6211138875,12.2812500009559,0.));
#5663=CARTESIAN_POINT('Ctrl Pts',(-1.6211138875,12.2229166676226,-0.935950539335166));
#5664=CARTESIAN_POINT('Ctrl Pts',(-0.81055694375,12.1645833342893,-1.40392580900275));
#5665=CARTESIAN_POINT('Ctrl Pts',(-1.14620883215705E-16,12.1062500009559,
-1.87190107867033));
#5666=CARTESIAN_POINT('Ctrl Pts',(0.81055694375,12.0479166676226,-1.40392580900275));
#5667=CARTESIAN_POINT('Ctrl Pts',(1.6211138875,11.9895833342893,-0.935950539335166));
#5668=CARTESIAN_POINT('Ctrl Pts',(1.6211138875,11.9312500009559,-1.9852919333802E-16));
#5669=CARTESIAN_POINT('Ctrl Pts',(1.6211138875,11.8729166676226,0.935950539335165));
#5670=CARTESIAN_POINT('Ctrl Pts',(0.810556943750001,11.8145833342893,1.40392580900275));
#5671=CARTESIAN_POINT('Ctrl Pts',(3.43862649647115E-16,11.7562500009559,
1.87190107867033));
#5672=CARTESIAN_POINT('Ctrl Pts',(-0.810556943749999,11.6979166676226,1.40392580900275));
#5673=CARTESIAN_POINT('Ctrl Pts',(-1.6211138875,11.6395833342893,0.935950539335167));
#5674=CARTESIAN_POINT('Ctrl Pts',(-1.6211138875,11.5812500009559,0.));
#5675=CARTESIAN_POINT('Ctrl Pts',(-1.6211138875,11.5229166676226,-0.935950539335166));
#5676=CARTESIAN_POINT('Ctrl Pts',(-0.81055694375,11.4645833342893,-1.40392580900275));
#5677=CARTESIAN_POINT('Ctrl Pts',(-1.14620883215705E-16,11.4062500009559,
-1.87190107867033));
#5678=CARTESIAN_POINT('Ctrl Pts',(0.81055694375,11.3479166676226,-1.40392580900275));
#5679=CARTESIAN_POINT('Ctrl Pts',(1.6211138875,11.2895833342893,-0.935950539335166));
#5680=CARTESIAN_POINT('Ctrl Pts',(1.6211138875,11.2312500009559,-1.9852919333802E-16));
#5681=CARTESIAN_POINT('Ctrl Pts',(1.6211138875,11.1729166676226,0.935950539335165));
#5682=CARTESIAN_POINT('Ctrl Pts',(0.810556943750001,11.1145833342893,1.40392580900275));
#5683=CARTESIAN_POINT('Ctrl Pts',(3.43862649647115E-16,11.0562500009559,
1.87190107867033));
#5684=CARTESIAN_POINT('Ctrl Pts',(-0.810556943749999,10.9979166676226,1.40392580900275));
#5685=CARTESIAN_POINT('Ctrl Pts',(-1.6211138875,10.9395833342893,0.935950539335167));
#5686=CARTESIAN_POINT('Ctrl Pts',(-1.6211138875,10.8812500009559,0.));
#5687=CARTESIAN_POINT('Ctrl Pts',(-1.6211138875,10.8229166676226,-0.935950539335166));
#5688=CARTESIAN_POINT('Ctrl Pts',(-0.81055694375,10.7645833342893,-1.40392580900275));
#5689=CARTESIAN_POINT('Ctrl Pts',(-1.14620883215705E-16,10.7062500009559,
-1.87190107867033));
#5690=CARTESIAN_POINT('Ctrl Pts',(0.81055694375,10.6479166676226,-1.40392580900275));
#5691=CARTESIAN_POINT('Ctrl Pts',(1.6211138875,10.5895833342893,-0.935950539335166));
#5692=CARTESIAN_POINT('Ctrl Pts',(1.6211138875,10.5312500009559,-1.9852919333802E-16));
#5693=CARTESIAN_POINT('Ctrl Pts',(1.6211138875,10.4729166676226,0.935950539335165));
#5694=CARTESIAN_POINT('Ctrl Pts',(0.810556943750001,10.4145833342893,1.40392580900275));
#5695=CARTESIAN_POINT('Ctrl Pts',(3.43862649647115E-16,10.3562500009559,
1.87190107867033));
#5696=CARTESIAN_POINT('Ctrl Pts',(-0.810556943749999,10.2979166676226,1.40392580900275));
#5697=CARTESIAN_POINT('Ctrl Pts',(-1.6211138875,10.2395833342893,0.935950539335167));
#5698=CARTESIAN_POINT('Ctrl Pts',(-1.6211138875,10.1812500009559,0.));
#5699=CARTESIAN_POINT('Ctrl Pts',(-1.6211138875,10.1229166676226,-0.935950539335166));
#5700=CARTESIAN_POINT('Ctrl Pts',(-0.81055694375,10.0645833342893,-1.40392580900275));
#5701=CARTESIAN_POINT('Ctrl Pts',(-1.14620883215705E-16,10.0062500009559,
-1.87190107867033));
#5702=CARTESIAN_POINT('Ctrl Pts',(0.81055694375,9.94791666762259,-1.40392580900275));
#5703=CARTESIAN_POINT('Ctrl Pts',(1.6211138875,9.88958333428926,-0.935950539335166));
#5704=CARTESIAN_POINT('Ctrl Pts',(1.6211138875,9.83125000095592,-1.9852919333802E-16));
#5705=CARTESIAN_POINT('Ctrl Pts',(1.6211138875,9.77291666762259,0.935950539335165));
#5706=CARTESIAN_POINT('Ctrl Pts',(0.810556943750001,9.71458333428926,1.40392580900275));
#5707=CARTESIAN_POINT('Ctrl Pts',(3.43862649647115E-16,9.65625000095592,
1.87190107867033));
#5708=CARTESIAN_POINT('Ctrl Pts',(-0.810556943749999,9.59791666762259,1.40392580900275));
#5709=CARTESIAN_POINT('Ctrl Pts',(-1.6211138875,9.53958333428925,0.935950539335167));
#5710=CARTESIAN_POINT('Ctrl Pts',(-1.6211138875,9.48125000095592,0.));
#5711=CARTESIAN_POINT('Ctrl Pts',(-1.6211138875,9.42291666762259,-0.935950539335166));
#5712=CARTESIAN_POINT('Ctrl Pts',(-0.81055694375,9.36458333428925,-1.40392580900275));
#5713=CARTESIAN_POINT('Ctrl Pts',(-1.14620883215705E-16,9.30625000095592,
-1.87190107867033));
#5714=CARTESIAN_POINT('Ctrl Pts',(0.81055694375,9.24791666762259,-1.40392580900275));
#5715=CARTESIAN_POINT('Ctrl Pts',(1.6211138875,9.18958333428925,-0.935950539335166));
#5716=CARTESIAN_POINT('Ctrl Pts',(1.6211138875,9.13125000095592,-1.9852919333802E-16));
#5717=CARTESIAN_POINT('Ctrl Pts',(1.6211138875,9.07291666762258,0.935950539335165));
#5718=CARTESIAN_POINT('Ctrl Pts',(0.810556943750001,9.01458333428926,1.40392580900275));
#5719=CARTESIAN_POINT('Ctrl Pts',(3.43862649647115E-16,8.95625000095592,
1.87190107867033));
#5720=CARTESIAN_POINT('Ctrl Pts',(-0.810556943749999,8.89791666762259,1.40392580900275));
#5721=CARTESIAN_POINT('Ctrl Pts',(-1.6211138875,8.83958333428926,0.935950539335167));
#5722=CARTESIAN_POINT('Ctrl Pts',(-1.6211138875,8.78125000095592,0.));
#5723=CARTESIAN_POINT('Ctrl Pts',(-1.6211138875,8.72291666762259,-0.935950539335166));
#5724=CARTESIAN_POINT('Ctrl Pts',(-0.81055694375,8.66458333428925,-1.40392580900275));
#5725=CARTESIAN_POINT('Ctrl Pts',(-1.14620883215705E-16,8.60625000095592,
-1.87190107867033));
#5726=CARTESIAN_POINT('Ctrl Pts',(0.81055694375,8.54791666762259,-1.40392580900275));
#5727=CARTESIAN_POINT('Ctrl Pts',(1.6211138875,8.48958333428926,-0.935950539335166));
#5728=CARTESIAN_POINT('Ctrl Pts',(1.6211138875,8.43125000095592,-1.9852919333802E-16));
#5729=CARTESIAN_POINT('Ctrl Pts',(1.6211138875,8.37291666762259,0.935950539335165));
#5730=CARTESIAN_POINT('Ctrl Pts',(0.810556943750001,8.31458333428925,1.40392580900275));
#5731=CARTESIAN_POINT('Ctrl Pts',(3.43862649647115E-16,8.25625000095592,
1.87190107867033));
#5732=CARTESIAN_POINT('Ctrl Pts',(-0.810556943749999,8.19791666762258,1.40392580900275));
#5733=CARTESIAN_POINT('Ctrl Pts',(-1.6211138875,8.13958333428925,0.935950539335167));
#5734=CARTESIAN_POINT('Ctrl Pts',(-1.6211138875,8.08125000095593,0.));
#5735=CARTESIAN_POINT('Ctrl Pts',(-1.6211138875,8.02291666762259,-0.935950539335166));
#5736=CARTESIAN_POINT('Ctrl Pts',(-0.81055694375,7.96458333428926,-1.40392580900275));
#5737=CARTESIAN_POINT('Ctrl Pts',(-1.14620883215705E-16,7.90625000095592,
-1.87190107867033));
#5738=CARTESIAN_POINT('Ctrl Pts',(0.81055694375,7.84791666762259,-1.40392580900275));
#5739=CARTESIAN_POINT('Ctrl Pts',(1.6211138875,7.78958333428925,-0.935950539335166));
#5740=CARTESIAN_POINT('Ctrl Pts',(1.6211138875,7.73125000095592,-1.9852919333802E-16));
#5741=CARTESIAN_POINT('Ctrl Pts',(1.6211138875,7.67291666762258,0.935950539335165));
#5742=CARTESIAN_POINT('Ctrl Pts',(0.810556943750001,7.61458333428926,1.40392580900275));
#5743=CARTESIAN_POINT('Ctrl Pts',(3.43862649647115E-16,7.55625000095592,
1.87190107867033));
#5744=CARTESIAN_POINT('Ctrl Pts',(-0.810556943749999,7.49791666762259,1.40392580900275));
#5745=CARTESIAN_POINT('Ctrl Pts',(-1.6211138875,7.43958333428925,0.935950539335167));
#5746=CARTESIAN_POINT('Ctrl Pts',(-1.6211138875,7.38125000095592,0.));
#5747=CARTESIAN_POINT('Ctrl Pts',(-1.6211138875,7.3229166676226,-0.935950539335166));
#5748=CARTESIAN_POINT('Ctrl Pts',(-0.81055694375,7.26458333428925,-1.40392580900275));
#5749=CARTESIAN_POINT('Ctrl Pts',(-1.14620883215705E-16,7.20625000095593,
-1.87190107867033));
#5750=CARTESIAN_POINT('Ctrl Pts',(0.81055694375,7.14791666762259,-1.40392580900275));
#5751=CARTESIAN_POINT('Ctrl Pts',(1.6211138875,7.08958333428926,-0.935950539335166));
#5752=CARTESIAN_POINT('Ctrl Pts',(1.6211138875,7.03125000095592,-1.9852919333802E-16));
#5753=CARTESIAN_POINT('Ctrl Pts',(1.6211138875,6.97291666762259,0.935950539335165));
#5754=CARTESIAN_POINT('Ctrl Pts',(0.810556943750001,6.91458333428925,1.40392580900275));
#5755=CARTESIAN_POINT('Ctrl Pts',(3.43862649647115E-16,6.85625000095592,
1.87190107867033));
#5756=CARTESIAN_POINT('Ctrl Pts',(-0.810556943749999,6.79791666762258,1.40392580900275));
#5757=CARTESIAN_POINT('Ctrl Pts',(-1.6211138875,6.73958333428926,0.935950539335167));
#5758=CARTESIAN_POINT('Ctrl Pts',(-1.6211138875,6.68125000095592,0.));
#5759=CARTESIAN_POINT('Ctrl Pts',(-1.6211138875,6.62291666762259,-0.935950539335166));
#5760=CARTESIAN_POINT('Ctrl Pts',(-0.81055694375,6.56458333428925,-1.40392580900275));
#5761=CARTESIAN_POINT('Ctrl Pts',(-1.14620883215705E-16,6.50625000095592,
-1.87190107867033));
#5762=CARTESIAN_POINT('Ctrl Pts',(0.81055694375,6.44791666762259,-1.40392580900275));
#5763=CARTESIAN_POINT('Ctrl Pts',(1.6211138875,6.38958333428925,-0.935950539335166));
#5764=CARTESIAN_POINT('Ctrl Pts',(1.6211138875,6.33125000095593,-1.9852919333802E-16));
#5765=CARTESIAN_POINT('Ctrl Pts',(1.6211138875,6.27291666762259,0.935950539335165));
#5766=CARTESIAN_POINT('Ctrl Pts',(0.810556943750001,6.21458333428926,1.40392580900275));
#5767=CARTESIAN_POINT('Ctrl Pts',(3.43862649647115E-16,6.15625000095592,
1.87190107867033));
#5768=CARTESIAN_POINT('Ctrl Pts',(-0.810556943749999,6.09791666762259,1.40392580900275));
#5769=CARTESIAN_POINT('Ctrl Pts',(-1.6211138875,6.03958333428925,0.935950539335167));
#5770=CARTESIAN_POINT('Ctrl Pts',(-1.6211138875,5.98125000095592,0.));
#5771=CARTESIAN_POINT('Ctrl Pts',(-1.6211138875,5.92291666762258,-0.935950539335166));
#5772=CARTESIAN_POINT('Ctrl Pts',(-0.81055694375,5.86458333428926,-1.40392580900275));
#5773=CARTESIAN_POINT('Ctrl Pts',(-1.14620883215705E-16,5.80625000095591,
-1.87190107867033));
#5774=CARTESIAN_POINT('Ctrl Pts',(0.81055694375,5.74791666762259,-1.40392580900275));
#5775=CARTESIAN_POINT('Ctrl Pts',(1.6211138875,5.68958333428926,-0.935950539335166));
#5776=CARTESIAN_POINT('Ctrl Pts',(1.6211138875,5.63125000095592,-1.9852919333802E-16));
#5777=CARTESIAN_POINT('Ctrl Pts',(1.6211138875,5.57291666762259,0.935950539335165));
#5778=CARTESIAN_POINT('Ctrl Pts',(0.810556943750001,5.51458333428925,1.40392580900275));
#5779=CARTESIAN_POINT('Ctrl Pts',(3.43862649647115E-16,5.45625000095593,
1.87190107867033));
#5780=CARTESIAN_POINT('Ctrl Pts',(-0.810556943749999,5.39791666762259,1.40392580900275));
#5781=CARTESIAN_POINT('Ctrl Pts',(-1.6211138875,5.33958333428926,0.935950539335167));
#5782=CARTESIAN_POINT('Ctrl Pts',(-1.6211138875,5.28125000095592,0.));
#5783=CARTESIAN_POINT('Ctrl Pts',(-1.6211138875,5.22291666762259,-0.935950539335166));
#5784=CARTESIAN_POINT('Ctrl Pts',(-0.81055694375,5.16458333428925,-1.40392580900275));
#5785=CARTESIAN_POINT('Ctrl Pts',(-1.14620883215705E-16,5.10625000095592,
-1.87190107867033));
#5786=CARTESIAN_POINT('Ctrl Pts',(0.81055694375,5.04791666762258,-1.40392580900275));
#5787=CARTESIAN_POINT('Ctrl Pts',(1.6211138875,4.98958333428925,-0.935950539335166));
#5788=CARTESIAN_POINT('Ctrl Pts',(1.6211138875,4.93125000095593,-1.9852919333802E-16));
#5789=CARTESIAN_POINT('Ctrl Pts',(1.6211138875,4.87291666762259,0.935950539335165));
#5790=CARTESIAN_POINT('Ctrl Pts',(0.810556943750001,4.81458333428926,1.40392580900275));
#5791=CARTESIAN_POINT('Ctrl Pts',(3.43862649647115E-16,4.75625000095592,
1.87190107867033));
#5792=CARTESIAN_POINT('Ctrl Pts',(-0.810556943749999,4.69791666762259,1.40392580900275));
#5793=CARTESIAN_POINT('Ctrl Pts',(-1.6211138875,4.63958333428925,0.935950539335167));
#5794=CARTESIAN_POINT('Ctrl Pts',(-1.6211138875,4.58125000095593,0.));
#5795=CARTESIAN_POINT('Ctrl Pts',(-1.6211138875,4.52291666762258,-0.935950539335166));
#5796=CARTESIAN_POINT('Ctrl Pts',(-0.81055694375,4.46458333428926,-1.40392580900275));
#5797=CARTESIAN_POINT('Ctrl Pts',(-1.14620883215705E-16,4.40625000095592,
-1.87190107867033));
#5798=CARTESIAN_POINT('Ctrl Pts',(0.81055694375,4.34791666762259,-1.40392580900275));
#5799=CARTESIAN_POINT('Ctrl Pts',(1.6211138875,4.28958333428925,-0.935950539335166));
#5800=CARTESIAN_POINT('Ctrl Pts',(1.6211138875,4.23125000095592,-1.9852919333802E-16));
#5801=CARTESIAN_POINT('Ctrl Pts',(1.6211138875,4.1729166676226,0.935950539335165));
#5802=CARTESIAN_POINT('Ctrl Pts',(0.810556943750001,4.11458333428925,1.40392580900275));
#5803=CARTESIAN_POINT('Ctrl Pts',(3.43862649647115E-16,4.05625000095593,
1.87190107867033));
#5804=CARTESIAN_POINT('Ctrl Pts',(-0.810556943749999,3.99791666762259,1.40392580900275));
#5805=CARTESIAN_POINT('Ctrl Pts',(-1.6211138875,3.93958333428926,0.935950539335167));
#5806=CARTESIAN_POINT('Ctrl Pts',(-1.6211138875,3.88125000095592,0.));
#5807=CARTESIAN_POINT('Ctrl Pts',(-1.6211138875,3.82291666762259,-0.935950539335166));
#5808=CARTESIAN_POINT('Ctrl Pts',(-0.81055694375,3.76458333428925,-1.40392580900275));
#5809=CARTESIAN_POINT('Ctrl Pts',(-1.14620883215705E-16,3.70625000095592,
-1.87190107867033));
#5810=CARTESIAN_POINT('Ctrl Pts',(0.81055694375,3.64791666762258,-1.40392580900275));
#5811=CARTESIAN_POINT('Ctrl Pts',(1.6211138875,3.58958333428926,-0.935950539335166));
#5812=CARTESIAN_POINT('Ctrl Pts',(1.6211138875,3.53125000095592,-1.9852919333802E-16));
#5813=CARTESIAN_POINT('Ctrl Pts',(1.6211138875,3.47291666762259,0.935950539335165));
#5814=CARTESIAN_POINT('Ctrl Pts',(0.810556943750001,3.41458333428925,1.40392580900275));
#5815=CARTESIAN_POINT('Ctrl Pts',(3.43862649647115E-16,3.35625000095592,
1.87190107867033));
#5816=CARTESIAN_POINT('Ctrl Pts',(-0.810556943749999,3.29791666762259,1.40392580900275));
#5817=CARTESIAN_POINT('Ctrl Pts',(-1.6211138875,3.23958333428925,0.935950539335167));
#5818=CARTESIAN_POINT('Ctrl Pts',(-1.6211138875,3.18125000095593,0.));
#5819=CARTESIAN_POINT('Ctrl Pts',(-1.6211138875,3.12291666762259,-0.935950539335166));
#5820=CARTESIAN_POINT('Ctrl Pts',(-0.81055694375,3.06458333428926,-1.40392580900275));
#5821=CARTESIAN_POINT('Ctrl Pts',(-1.14620883215705E-16,3.00625000095592,
-1.87190107867033));
#5822=CARTESIAN_POINT('Ctrl Pts',(0.81055694375,2.94791666762259,-1.40392580900275));
#5823=CARTESIAN_POINT('Ctrl Pts',(1.6211138875,2.88958333428925,-0.935950539335166));
#5824=CARTESIAN_POINT('Ctrl Pts',(1.6211138875,2.83125000095592,-1.9852919333802E-16));
#5825=CARTESIAN_POINT('Ctrl Pts',(1.6211138875,2.77291666762258,0.935950539335165));
#5826=CARTESIAN_POINT('Ctrl Pts',(0.810556943750001,2.71458333428926,1.40392580900275));
#5827=CARTESIAN_POINT('Ctrl Pts',(3.43862649647115E-16,2.65625000095591,
1.87190107867033));
#5828=CARTESIAN_POINT('Ctrl Pts',(-0.810556943749999,2.59791666762259,1.40392580900275));
#5829=CARTESIAN_POINT('Ctrl Pts',(-1.6211138875,2.53958333428926,0.935950539335167));
#5830=CARTESIAN_POINT('Ctrl Pts',(-1.6211138875,2.48125000095592,0.));
#5831=CARTESIAN_POINT('Ctrl Pts',(-1.6211138875,2.42291666762259,-0.935950539335166));
#5832=CARTESIAN_POINT('Ctrl Pts',(-0.81055694375,2.36458333428925,-1.40392580900275));
#5833=CARTESIAN_POINT('Ctrl Pts',(-1.14620883215705E-16,2.30625000095593,
-1.87190107867033));
#5834=CARTESIAN_POINT('Ctrl Pts',(0.81055694375,2.24791666762258,-1.40392580900275));
#5835=CARTESIAN_POINT('Ctrl Pts',(1.6211138875,2.18958333428926,-0.935950539335166));
#5836=CARTESIAN_POINT('Ctrl Pts',(1.6211138875,2.13125000095592,-1.9852919333802E-16));
#5837=CARTESIAN_POINT('Ctrl Pts',(1.6211138875,2.07291666762259,0.935950539335165));
#5838=CARTESIAN_POINT('Ctrl Pts',(0.810556943750001,2.01458333428925,1.40392580900275));
#5839=CARTESIAN_POINT('Ctrl Pts',(3.43862649647115E-16,1.95625000095592,
1.87190107867033));
#5840=CARTESIAN_POINT('Ctrl Pts',(-0.810556943749999,1.89791666762258,1.40392580900275));
#5841=CARTESIAN_POINT('Ctrl Pts',(-1.6211138875,1.83958333428925,0.935950539335167));
#5842=CARTESIAN_POINT('Ctrl Pts',(-1.6211138875,1.78125000095593,0.));
#5843=CARTESIAN_POINT('Ctrl Pts',(-1.6211138875,1.72291666762259,-0.935950539335166));
#5844=CARTESIAN_POINT('Ctrl Pts',(-0.81055694375,1.66458333428926,-1.40392580900275));
#5845=CARTESIAN_POINT('Ctrl Pts',(-1.14620883215705E-16,1.60625000095592,
-1.87190107867033));
#5846=CARTESIAN_POINT('Ctrl Pts',(0.81055694375,1.54791666762259,-1.40392580900275));
#5847=CARTESIAN_POINT('Ctrl Pts',(1.6211138875,1.48958333428925,-0.935950539335166));
#5848=CARTESIAN_POINT('Ctrl Pts',(1.6211138875,1.43125000095592,-1.9852919333802E-16));
#5849=CARTESIAN_POINT('Ctrl Pts',(1.6211138875,1.37291666762258,0.935950539335165));
#5850=CARTESIAN_POINT('Ctrl Pts',(0.810556943750001,1.31458333428926,1.40392580900275));
#5851=CARTESIAN_POINT('Ctrl Pts',(3.43862649647115E-16,1.25625000095592,
1.87190107867033));
#5852=CARTESIAN_POINT('Ctrl Pts',(-0.810556943749999,1.19791666762259,1.40392580900275));
#5853=CARTESIAN_POINT('Ctrl Pts',(-1.6211138875,1.13958333428925,0.935950539335167));
#5854=CARTESIAN_POINT('Ctrl Pts',(-1.6211138875,1.08125000095592,0.));
#5855=CARTESIAN_POINT('Ctrl Pts',(-1.6211138875,1.02291666762259,-0.935950539335166));
#5856=CARTESIAN_POINT('Ctrl Pts',(-0.81055694375,0.964583334289254,-1.40392580900275));
#5857=CARTESIAN_POINT('Ctrl Pts',(-1.14620883215705E-16,0.906250000955927,
-1.87190107867033));
#5858=CARTESIAN_POINT('Ctrl Pts',(0.81055694375,0.847916667622586,-1.40392580900275));
#5859=CARTESIAN_POINT('Ctrl Pts',(1.6211138875,0.789583334289259,-0.935950539335166));
#5860=CARTESIAN_POINT('Ctrl Pts',(1.6211138875,0.731250000955919,-1.9852919333802E-16));
#5861=CARTESIAN_POINT('Ctrl Pts',(1.6211138875,0.672916667622592,0.935950539335165));
#5862=CARTESIAN_POINT('Ctrl Pts',(0.810556943750001,0.614583334289251,1.40392580900275));
#5863=CARTESIAN_POINT('Ctrl Pts',(3.43862649647115E-16,0.556250000955924,
1.87190107867033));
#5864=CARTESIAN_POINT('Ctrl Pts',(-0.810556943749999,0.497916667622583,
1.40392580900275));
#5865=CARTESIAN_POINT('Ctrl Pts',(-1.6211138875,0.439583334289256,0.935950539335167));
#5866=CARTESIAN_POINT('Ctrl Pts',(-1.6211138875,0.381250000955916,0.));
#5867=CARTESIAN_POINT('Ctrl Pts',(-1.6211138875,0.322916667622589,-0.935950539335166));
#5868=CARTESIAN_POINT('Ctrl Pts',(-0.81055694375,0.264583334289248,-1.40392580900275));
#5869=CARTESIAN_POINT('Ctrl Pts',(-1.14620883215705E-16,0.206250000955921,
-1.87190107867033));
#5870=CARTESIAN_POINT('Ctrl Pts',(0.81055694375,0.147916667622594,-1.40392580900275));
#5871=CARTESIAN_POINT('Ctrl Pts',(1.6211138875,0.0895833342892532,-0.935950539335166));
#5872=CARTESIAN_POINT('Ctrl Pts',(1.6211138875,0.0312500009559263,-1.9852919333802E-16));
#5873=CARTESIAN_POINT('Ctrl Pts',(1.6211138875,-0.0270833323774144,0.935950539335165));
#5874=CARTESIAN_POINT('Ctrl Pts',(0.810556943750001,-0.0854166657107414,
1.40392580900275));
#5875=CARTESIAN_POINT('Ctrl Pts',(3.43862649647115E-16,-0.143749999044082,
1.87190107867033));
#5876=CARTESIAN_POINT('Ctrl Pts',(-0.810556943749999,-0.202083332377409,
1.40392580900275));
#5877=CARTESIAN_POINT('Ctrl Pts',(-1.6211138875,-0.26041666571075,0.935950539335167));
#5878=CARTESIAN_POINT('Ctrl Pts',(-1.6211138875,-0.318749999044077,0.));
#5879=CARTESIAN_POINT('Ctrl Pts',(-1.6211138875,-0.377083332377417,-0.935950539335166));
#5880=CARTESIAN_POINT('Ctrl Pts',(-0.81055694375,-0.435416665710744,-1.40392580900275));
#5881=CARTESIAN_POINT('Ctrl Pts',(-1.14620883215705E-16,-0.493749999044085,
-1.87190107867033));
#5882=CARTESIAN_POINT('Ctrl Pts',(0.81055694375,-0.552083332377412,-1.40392580900275));
#5883=CARTESIAN_POINT('Ctrl Pts',(1.6211138875,-0.610416665710739,-0.935950539335166));
#5884=CARTESIAN_POINT('Ctrl Pts',(1.6211138875,-0.66874999904408,-1.9852919333802E-16));
#5885=CARTESIAN_POINT('Ctrl Pts',(1.6211138875,-0.727083332377407,0.935950539335165));
#5886=CARTESIAN_POINT('Ctrl Pts',(0.810556943750001,-0.785416665710748,
1.40392580900275));
#5887=CARTESIAN_POINT('Ctrl Pts',(3.43862649647115E-16,-0.843749999044074,
1.87190107867033));
#5888=CARTESIAN_POINT('Ctrl Pts',(-0.810556943749999,-0.902083332377415,
1.40392580900275));
#5889=CARTESIAN_POINT('Ctrl Pts',(-1.6211138875,-0.960416665710742,0.935950539335167));
#5890=CARTESIAN_POINT('Ctrl Pts',(-1.6211138875,-1.01874999904408,0.));
#5891=CARTESIAN_POINT('Ctrl Pts',(-1.6211138875,-1.07708333237741,-0.935950539335166));
#5892=CARTESIAN_POINT('Ctrl Pts',(-0.81055694375,-1.13541666571075,-1.40392580900275));
#5893=CARTESIAN_POINT('Ctrl Pts',(-1.14620883215705E-16,-1.19374999904408,
-1.87190107867033));
#5894=CARTESIAN_POINT('Ctrl Pts',(0.81055694375,-1.25208333237742,-1.40392580900275));
#5895=CARTESIAN_POINT('Ctrl Pts',(1.6211138875,-1.31041666571075,-0.935950539335166));
#5896=CARTESIAN_POINT('Ctrl Pts',(1.6211138875,-1.36874999904407,-1.9852919333802E-16));
#5897=CARTESIAN_POINT('Ctrl Pts',(1.6211138875,-1.42708333237741,0.935950539335165));
#5898=CARTESIAN_POINT('Ctrl Pts',(0.810556943750001,-1.48541666571074,1.40392580900275));
#5899=CARTESIAN_POINT('Ctrl Pts',(3.43862649647115E-16,-1.54374999904408,
1.87190107867033));
#5900=CARTESIAN_POINT('Ctrl Pts',(-0.810556943749999,-1.60208333237741,
1.40392580900275));
#5901=CARTESIAN_POINT('Ctrl Pts',(-1.6211138875,-1.66041666571075,0.935950539335167));
#5902=CARTESIAN_POINT('Ctrl Pts',(-1.6211138875,-1.71874999904408,0.));
#5903=CARTESIAN_POINT('Ctrl Pts',(-1.6211138875,-1.77708333237742,-0.935950539335166));
#5904=CARTESIAN_POINT('Ctrl Pts',(-0.81055694375,-1.83541666571074,-1.40392580900275));
#5905=CARTESIAN_POINT('Ctrl Pts',(-1.14620883215705E-16,-1.89374999904408,
-1.87190107867033));
#5906=CARTESIAN_POINT('Ctrl Pts',(0.81055694375,-1.95208333237741,-1.40392580900275));
#5907=CARTESIAN_POINT('Ctrl Pts',(1.6211138875,-2.01041666571075,-0.935950539335166));
#5908=CARTESIAN_POINT('Ctrl Pts',(1.6211138875,-2.06874999904408,-1.9852919333802E-16));
#5909=CARTESIAN_POINT('Ctrl Pts',(1.6211138875,-2.12708333237741,0.935950539335165));
#5910=CARTESIAN_POINT('Ctrl Pts',(0.810556943750001,-2.18541666571075,1.40392580900275));
#5911=CARTESIAN_POINT('Ctrl Pts',(0.598919469048119,-2.20064757509077,1.52611476199249));
#5912=CARTESIAN_POINT('Ctrl Pts',(0.360666377423904,-2.217793929975,1.58048410319158));
#5913=CARTESIAN_POINT('Ctrl Pts',(-2.00000000049539,72.000000000286,0.));
#5914=CARTESIAN_POINT('Ctrl Pts',(-2.00000000049539,71.9416666669527,-1.15470053866527));
#5915=CARTESIAN_POINT('Ctrl Pts',(-1.0000000002477,71.8833333336194,-1.7320508079979));
#5916=CARTESIAN_POINT('Ctrl Pts',(-1.41410031865014E-16,71.825000000286,
-2.30940107733053));
#5917=CARTESIAN_POINT('Ctrl Pts',(1.0000000002477,71.7666666669527,-1.7320508079979));
#5918=CARTESIAN_POINT('Ctrl Pts',(2.00000000049539,71.7083333336194,-1.15470053866527));
#5919=CARTESIAN_POINT('Ctrl Pts',(2.00000000049539,71.650000000286,-2.44929359890139E-16));
#5920=CARTESIAN_POINT('Ctrl Pts',(2.00000000049539,71.5916666669527,1.15470053866527));
#5921=CARTESIAN_POINT('Ctrl Pts',(1.0000000002477,71.5333333336193,1.7320508079979));
#5922=CARTESIAN_POINT('Ctrl Pts',(4.24230095595043E-16,71.475000000286,
2.30940107733053));
#5923=CARTESIAN_POINT('Ctrl Pts',(-1.0000000002477,71.4166666669527,1.7320508079979));
#5924=CARTESIAN_POINT('Ctrl Pts',(-2.00000000049539,71.3583333336194,1.15470053866527));
#5925=CARTESIAN_POINT('Ctrl Pts',(-2.00000000049539,71.300000000286,0.));
#5926=CARTESIAN_POINT('Ctrl Pts',(-2.00000000049539,71.2416666669527,-1.15470053866527));
#5927=CARTESIAN_POINT('Ctrl Pts',(-1.0000000002477,71.1833333336194,-1.7320508079979));
#5928=CARTESIAN_POINT('Ctrl Pts',(-1.41410031865014E-16,71.125000000286,
-2.30940107733053));
#5929=CARTESIAN_POINT('Ctrl Pts',(1.0000000002477,71.0666666669527,-1.7320508079979));
#5930=CARTESIAN_POINT('Ctrl Pts',(2.00000000049539,71.0083333336193,-1.15470053866527));
#5931=CARTESIAN_POINT('Ctrl Pts',(2.00000000049539,70.950000000286,-2.44929359890139E-16));
#5932=CARTESIAN_POINT('Ctrl Pts',(2.00000000049539,70.8916666669527,1.15470053866527));
#5933=CARTESIAN_POINT('Ctrl Pts',(1.0000000002477,70.8333333336194,1.7320508079979));
#5934=CARTESIAN_POINT('Ctrl Pts',(4.24230095595043E-16,70.775000000286,
2.30940107733053));
#5935=CARTESIAN_POINT('Ctrl Pts',(-1.0000000002477,70.7166666669527,1.7320508079979));
#5936=CARTESIAN_POINT('Ctrl Pts',(-2.00000000049539,70.6583333336194,1.15470053866527));
#5937=CARTESIAN_POINT('Ctrl Pts',(-2.00000000049539,70.600000000286,0.));
#5938=CARTESIAN_POINT('Ctrl Pts',(-2.00000000049539,70.5416666669527,-1.15470053866527));
#5939=CARTESIAN_POINT('Ctrl Pts',(-1.0000000002477,70.4833333336194,-1.7320508079979));
#5940=CARTESIAN_POINT('Ctrl Pts',(-1.41410031865014E-16,70.425000000286,
-2.30940107733053));
#5941=CARTESIAN_POINT('Ctrl Pts',(1.0000000002477,70.3666666669527,-1.7320508079979));
#5942=CARTESIAN_POINT('Ctrl Pts',(2.00000000049539,70.3083333336194,-1.15470053866527));
#5943=CARTESIAN_POINT('Ctrl Pts',(2.00000000049539,70.250000000286,-2.44929359890139E-16));
#5944=CARTESIAN_POINT('Ctrl Pts',(2.00000000049539,70.1916666669527,1.15470053866527));
#5945=CARTESIAN_POINT('Ctrl Pts',(1.0000000002477,70.1333333336194,1.7320508079979));
#5946=CARTESIAN_POINT('Ctrl Pts',(4.24230095595043E-16,70.075000000286,
2.30940107733053));
#5947=CARTESIAN_POINT('Ctrl Pts',(-1.0000000002477,70.0166666669527,1.7320508079979));
#5948=CARTESIAN_POINT('Ctrl Pts',(-2.00000000049539,69.9583333336194,1.15470053866527));
#5949=CARTESIAN_POINT('Ctrl Pts',(-2.00000000049539,69.900000000286,0.));
#5950=CARTESIAN_POINT('Ctrl Pts',(-2.00000000049539,69.8416666669527,-1.15470053866527));
#5951=CARTESIAN_POINT('Ctrl Pts',(-1.0000000002477,69.7833333336193,-1.7320508079979));
#5952=CARTESIAN_POINT('Ctrl Pts',(-1.41410031865014E-16,69.725000000286,
-2.30940107733053));
#5953=CARTESIAN_POINT('Ctrl Pts',(1.0000000002477,69.6666666669527,-1.7320508079979));
#5954=CARTESIAN_POINT('Ctrl Pts',(2.00000000049539,69.6083333336193,-1.15470053866527));
#5955=CARTESIAN_POINT('Ctrl Pts',(2.00000000049539,69.550000000286,-2.44929359890139E-16));
#5956=CARTESIAN_POINT('Ctrl Pts',(2.00000000049539,69.4916666669527,1.15470053866527));
#5957=CARTESIAN_POINT('Ctrl Pts',(1.0000000002477,69.4333333336194,1.7320508079979));
#5958=CARTESIAN_POINT('Ctrl Pts',(4.24230095595043E-16,69.375000000286,
2.30940107733053));
#5959=CARTESIAN_POINT('Ctrl Pts',(-1.0000000002477,69.3166666669527,1.7320508079979));
#5960=CARTESIAN_POINT('Ctrl Pts',(-2.00000000049539,69.2583333336193,1.15470053866527));
#5961=CARTESIAN_POINT('Ctrl Pts',(-2.00000000049539,69.200000000286,0.));
#5962=CARTESIAN_POINT('Ctrl Pts',(-2.00000000049539,69.1416666669527,-1.15470053866527));
#5963=CARTESIAN_POINT('Ctrl Pts',(-1.0000000002477,69.0833333336194,-1.7320508079979));
#5964=CARTESIAN_POINT('Ctrl Pts',(-1.41410031865014E-16,69.025000000286,
-2.30940107733053));
#5965=CARTESIAN_POINT('Ctrl Pts',(1.0000000002477,68.9666666669527,-1.7320508079979));
#5966=CARTESIAN_POINT('Ctrl Pts',(2.00000000049539,68.9083333336194,-1.15470053866527));
#5967=CARTESIAN_POINT('Ctrl Pts',(2.00000000049539,68.850000000286,-2.44929359890139E-16));
#5968=CARTESIAN_POINT('Ctrl Pts',(2.00000000049539,68.7916666669527,1.15470053866527));
#5969=CARTESIAN_POINT('Ctrl Pts',(1.0000000002477,68.7333333336194,1.7320508079979));
#5970=CARTESIAN_POINT('Ctrl Pts',(4.24230095595043E-16,68.675000000286,
2.30940107733053));
#5971=CARTESIAN_POINT('Ctrl Pts',(-1.0000000002477,68.6166666669527,1.7320508079979));
#5972=CARTESIAN_POINT('Ctrl Pts',(-2.00000000049539,68.5583333336194,1.15470053866527));
#5973=CARTESIAN_POINT('Ctrl Pts',(-2.00000000049539,68.500000000286,0.));
#5974=CARTESIAN_POINT('Ctrl Pts',(-2.00000000049539,68.4416666669527,-1.15470053866527));
#5975=CARTESIAN_POINT('Ctrl Pts',(-1.0000000002477,68.3833333336194,-1.7320508079979));
#5976=CARTESIAN_POINT('Ctrl Pts',(-1.41410031865014E-16,68.325000000286,
-2.30940107733053));
#5977=CARTESIAN_POINT('Ctrl Pts',(1.0000000002477,68.2666666669527,-1.7320508079979));
#5978=CARTESIAN_POINT('Ctrl Pts',(2.00000000049539,68.2083333336194,-1.15470053866527));
#5979=CARTESIAN_POINT('Ctrl Pts',(2.00000000049539,68.150000000286,-2.44929359890139E-16));
#5980=CARTESIAN_POINT('Ctrl Pts',(2.00000000049539,68.0916666669527,1.15470053866527));
#5981=CARTESIAN_POINT('Ctrl Pts',(1.0000000002477,68.0333333336194,1.7320508079979));
#5982=CARTESIAN_POINT('Ctrl Pts',(4.24230095595043E-16,67.975000000286,
2.30940107733053));
#5983=CARTESIAN_POINT('Ctrl Pts',(-1.0000000002477,67.9166666669527,1.7320508079979));
#5984=CARTESIAN_POINT('Ctrl Pts',(-2.00000000049539,67.8583333336194,1.15470053866527));
#5985=CARTESIAN_POINT('Ctrl Pts',(-2.00000000049539,67.800000000286,0.));
#5986=CARTESIAN_POINT('Ctrl Pts',(-2.00000000049539,67.7416666669527,-1.15470053866527));
#5987=CARTESIAN_POINT('Ctrl Pts',(-1.0000000002477,67.6833333336194,-1.7320508079979));
#5988=CARTESIAN_POINT('Ctrl Pts',(-1.41410031865014E-16,67.625000000286,
-2.30940107733053));
#5989=CARTESIAN_POINT('Ctrl Pts',(1.0000000002477,67.5666666669527,-1.7320508079979));
#5990=CARTESIAN_POINT('Ctrl Pts',(2.00000000049539,67.5083333336193,-1.15470053866527));
#5991=CARTESIAN_POINT('Ctrl Pts',(2.00000000049539,67.450000000286,-2.44929359890139E-16));
#5992=CARTESIAN_POINT('Ctrl Pts',(2.00000000049539,67.3916666669527,1.15470053866527));
#5993=CARTESIAN_POINT('Ctrl Pts',(1.0000000002477,67.3333333336194,1.7320508079979));
#5994=CARTESIAN_POINT('Ctrl Pts',(4.24230095595043E-16,67.275000000286,
2.30940107733053));
#5995=CARTESIAN_POINT('Ctrl Pts',(-1.0000000002477,67.2166666669527,1.7320508079979));
#5996=CARTESIAN_POINT('Ctrl Pts',(-2.00000000049539,67.1583333336194,1.15470053866527));
#5997=CARTESIAN_POINT('Ctrl Pts',(-2.00000000049539,67.100000000286,0.));
#5998=CARTESIAN_POINT('Ctrl Pts',(-2.00000000049539,67.0416666669527,-1.15470053866527));
#5999=CARTESIAN_POINT('Ctrl Pts',(-1.0000000002477,66.9833333336194,-1.7320508079979));
#6000=CARTESIAN_POINT('Ctrl Pts',(-1.41410031865014E-16,66.925000000286,
-2.30940107733053));
#6001=CARTESIAN_POINT('Ctrl Pts',(1.0000000002477,66.8666666669527,-1.7320508079979));
#6002=CARTESIAN_POINT('Ctrl Pts',(2.00000000049539,66.8083333336194,-1.15470053866527));
#6003=CARTESIAN_POINT('Ctrl Pts',(2.00000000049539,66.750000000286,-2.44929359890139E-16));
#6004=CARTESIAN_POINT('Ctrl Pts',(2.00000000049539,66.6916666669527,1.15470053866527));
#6005=CARTESIAN_POINT('Ctrl Pts',(1.0000000002477,66.6333333336194,1.7320508079979));
#6006=CARTESIAN_POINT('Ctrl Pts',(4.24230095595043E-16,66.575000000286,
2.30940107733053));
#6007=CARTESIAN_POINT('Ctrl Pts',(-1.0000000002477,66.5166666669527,1.7320508079979));
#6008=CARTESIAN_POINT('Ctrl Pts',(-2.00000000049539,66.4583333336194,1.15470053866527));
#6009=CARTESIAN_POINT('Ctrl Pts',(-2.00000000049539,66.400000000286,0.));
#6010=CARTESIAN_POINT('Ctrl Pts',(-2.00000000049539,66.3416666669527,-1.15470053866527));
#6011=CARTESIAN_POINT('Ctrl Pts',(-1.0000000002477,66.2833333336194,-1.7320508079979));
#6012=CARTESIAN_POINT('Ctrl Pts',(-1.41410031865014E-16,66.225000000286,
-2.30940107733053));
#6013=CARTESIAN_POINT('Ctrl Pts',(1.0000000002477,66.1666666669527,-1.7320508079979));
#6014=CARTESIAN_POINT('Ctrl Pts',(2.00000000049539,66.1083333336194,-1.15470053866527));
#6015=CARTESIAN_POINT('Ctrl Pts',(2.00000000049539,66.050000000286,-2.44929359890139E-16));
#6016=CARTESIAN_POINT('Ctrl Pts',(2.00000000049539,65.9916666669527,1.15470053866527));
#6017=CARTESIAN_POINT('Ctrl Pts',(1.0000000002477,65.9333333336193,1.7320508079979));
#6018=CARTESIAN_POINT('Ctrl Pts',(4.24230095595043E-16,65.875000000286,
2.30940107733053));
#6019=CARTESIAN_POINT('Ctrl Pts',(-1.0000000002477,65.8166666669527,1.7320508079979));
#6020=CARTESIAN_POINT('Ctrl Pts',(-2.00000000049539,65.7583333336193,1.15470053866527));
#6021=CARTESIAN_POINT('Ctrl Pts',(-2.00000000049539,65.700000000286,0.));
#6022=CARTESIAN_POINT('Ctrl Pts',(-2.00000000049539,65.6416666669527,-1.15470053866527));
#6023=CARTESIAN_POINT('Ctrl Pts',(-1.0000000002477,65.5833333336194,-1.7320508079979));
#6024=CARTESIAN_POINT('Ctrl Pts',(-1.41410031865014E-16,65.525000000286,
-2.30940107733053));
#6025=CARTESIAN_POINT('Ctrl Pts',(1.0000000002477,65.4666666669527,-1.7320508079979));
#6026=CARTESIAN_POINT('Ctrl Pts',(2.00000000049539,65.4083333336194,-1.15470053866527));
#6027=CARTESIAN_POINT('Ctrl Pts',(2.00000000049539,65.350000000286,-2.44929359890139E-16));
#6028=CARTESIAN_POINT('Ctrl Pts',(2.00000000049539,65.2916666669527,1.15470053866527));
#6029=CARTESIAN_POINT('Ctrl Pts',(1.0000000002477,65.2333333336193,1.7320508079979));
#6030=CARTESIAN_POINT('Ctrl Pts',(4.24230095595043E-16,65.175000000286,
2.30940107733053));
#6031=CARTESIAN_POINT('Ctrl Pts',(-1.0000000002477,65.1166666669527,1.7320508079979));
#6032=CARTESIAN_POINT('Ctrl Pts',(-2.00000000049539,65.0583333336194,1.15470053866527));
#6033=CARTESIAN_POINT('Ctrl Pts',(-2.00000000049539,65.000000000286,0.));
#6034=CARTESIAN_POINT('Ctrl Pts',(-2.00000000049539,64.9416666669527,-1.15470053866527));
#6035=CARTESIAN_POINT('Ctrl Pts',(-1.0000000002477,64.8833333336194,-1.7320508079979));
#6036=CARTESIAN_POINT('Ctrl Pts',(-1.41410031865014E-16,64.825000000286,
-2.30940107733053));
#6037=CARTESIAN_POINT('Ctrl Pts',(1.0000000002477,64.7666666669527,-1.7320508079979));
#6038=CARTESIAN_POINT('Ctrl Pts',(2.00000000049539,64.7083333336194,-1.15470053866527));
#6039=CARTESIAN_POINT('Ctrl Pts',(2.00000000049539,64.650000000286,-2.44929359890139E-16));
#6040=CARTESIAN_POINT('Ctrl Pts',(2.00000000049539,64.5916666669527,1.15470053866527));
#6041=CARTESIAN_POINT('Ctrl Pts',(1.0000000002477,64.5333333336194,1.7320508079979));
#6042=CARTESIAN_POINT('Ctrl Pts',(4.24230095595043E-16,64.475000000286,
2.30940107733053));
#6043=CARTESIAN_POINT('Ctrl Pts',(-1.0000000002477,64.4166666669527,1.7320508079979));
#6044=CARTESIAN_POINT('Ctrl Pts',(-2.00000000049539,64.3583333336194,1.15470053866527));
#6045=CARTESIAN_POINT('Ctrl Pts',(-2.00000000049539,64.300000000286,0.));
#6046=CARTESIAN_POINT('Ctrl Pts',(-2.00000000049539,64.2416666669527,-1.15470053866527));
#6047=CARTESIAN_POINT('Ctrl Pts',(-1.0000000002477,64.1833333336193,-1.7320508079979));
#6048=CARTESIAN_POINT('Ctrl Pts',(-1.41410031865014E-16,64.125000000286,
-2.30940107733053));
#6049=CARTESIAN_POINT('Ctrl Pts',(1.0000000002477,64.0666666669527,-1.7320508079979));
#6050=CARTESIAN_POINT('Ctrl Pts',(2.00000000049539,64.0083333336194,-1.15470053866527));
#6051=CARTESIAN_POINT('Ctrl Pts',(2.00000000049539,63.950000000286,-2.44929359890139E-16));
#6052=CARTESIAN_POINT('Ctrl Pts',(2.00000000049539,63.8916666669527,1.15470053866527));
#6053=CARTESIAN_POINT('Ctrl Pts',(1.0000000002477,63.8333333336194,1.7320508079979));
#6054=CARTESIAN_POINT('Ctrl Pts',(4.24230095595043E-16,63.775000000286,
2.30940107733053));
#6055=CARTESIAN_POINT('Ctrl Pts',(-1.0000000002477,63.7166666669527,1.7320508079979));
#6056=CARTESIAN_POINT('Ctrl Pts',(-2.00000000049539,63.6583333336194,1.15470053866527));
#6057=CARTESIAN_POINT('Ctrl Pts',(-2.00000000049539,63.600000000286,0.));
#6058=CARTESIAN_POINT('Ctrl Pts',(-2.00000000049539,63.5416666669527,-1.15470053866527));
#6059=CARTESIAN_POINT('Ctrl Pts',(-1.0000000002477,63.4833333336193,-1.7320508079979));
#6060=CARTESIAN_POINT('Ctrl Pts',(-1.41410031865014E-16,63.425000000286,
-2.30940107733053));
#6061=CARTESIAN_POINT('Ctrl Pts',(1.0000000002477,63.3666666669527,-1.7320508079979));
#6062=CARTESIAN_POINT('Ctrl Pts',(2.00000000049539,63.3083333336194,-1.15470053866527));
#6063=CARTESIAN_POINT('Ctrl Pts',(2.00000000049539,63.250000000286,-2.44929359890139E-16));
#6064=CARTESIAN_POINT('Ctrl Pts',(2.00000000049539,63.1916666669527,1.15470053866527));
#6065=CARTESIAN_POINT('Ctrl Pts',(1.0000000002477,63.1333333336194,1.7320508079979));
#6066=CARTESIAN_POINT('Ctrl Pts',(4.24230095595043E-16,63.075000000286,
2.30940107733053));
#6067=CARTESIAN_POINT('Ctrl Pts',(-1.0000000002477,63.0166666669527,1.7320508079979));
#6068=CARTESIAN_POINT('Ctrl Pts',(-2.00000000049539,62.9583333336194,1.15470053866527));
#6069=CARTESIAN_POINT('Ctrl Pts',(-2.00000000049539,62.900000000286,0.));
#6070=CARTESIAN_POINT('Ctrl Pts',(-2.00000000049539,62.8416666669527,-1.15470053866527));
#6071=CARTESIAN_POINT('Ctrl Pts',(-1.0000000002477,62.7833333336194,-1.7320508079979));
#6072=CARTESIAN_POINT('Ctrl Pts',(-1.41410031865014E-16,62.725000000286,
-2.30940107733053));
#6073=CARTESIAN_POINT('Ctrl Pts',(1.0000000002477,62.6666666669527,-1.7320508079979));
#6074=CARTESIAN_POINT('Ctrl Pts',(2.00000000049539,62.6083333336194,-1.15470053866527));
#6075=CARTESIAN_POINT('Ctrl Pts',(2.00000000049539,62.550000000286,-2.44929359890139E-16));
#6076=CARTESIAN_POINT('Ctrl Pts',(2.00000000049539,62.4916666669527,1.15470053866527));
#6077=CARTESIAN_POINT('Ctrl Pts',(1.0000000002477,62.4333333336194,1.7320508079979));
#6078=CARTESIAN_POINT('Ctrl Pts',(4.24230095595043E-16,62.375000000286,
2.30940107733053));
#6079=CARTESIAN_POINT('Ctrl Pts',(-1.0000000002477,62.3166666669527,1.7320508079979));
#6080=CARTESIAN_POINT('Ctrl Pts',(-2.00000000049539,62.2583333336194,1.15470053866527));
#6081=CARTESIAN_POINT('Ctrl Pts',(-2.00000000049539,62.200000000286,0.));
#6082=CARTESIAN_POINT('Ctrl Pts',(-2.00000000049539,62.1416666669527,-1.15470053866527));
#6083=CARTESIAN_POINT('Ctrl Pts',(-1.0000000002477,62.0833333336194,-1.7320508079979));
#6084=CARTESIAN_POINT('Ctrl Pts',(-1.41410031865014E-16,62.025000000286,
-2.30940107733053));
#6085=CARTESIAN_POINT('Ctrl Pts',(1.0000000002477,61.9666666669527,-1.7320508079979));
#6086=CARTESIAN_POINT('Ctrl Pts',(2.00000000049539,61.9083333336194,-1.15470053866527));
#6087=CARTESIAN_POINT('Ctrl Pts',(2.00000000049539,61.850000000286,-2.44929359890139E-16));
#6088=CARTESIAN_POINT('Ctrl Pts',(2.00000000049539,61.7916666669527,1.15470053866527));
#6089=CARTESIAN_POINT('Ctrl Pts',(1.0000000002477,61.7333333336194,1.7320508079979));
#6090=CARTESIAN_POINT('Ctrl Pts',(4.24230095595043E-16,61.675000000286,
2.30940107733053));
#6091=CARTESIAN_POINT('Ctrl Pts',(-1.0000000002477,61.6166666669527,1.7320508079979));
#6092=CARTESIAN_POINT('Ctrl Pts',(-2.00000000049539,61.5583333336193,1.15470053866527));
#6093=CARTESIAN_POINT('Ctrl Pts',(-2.00000000049539,61.500000000286,0.));
#6094=CARTESIAN_POINT('Ctrl Pts',(-2.00000000049539,61.4416666669527,-1.15470053866527));
#6095=CARTESIAN_POINT('Ctrl Pts',(-1.0000000002477,61.3833333336194,-1.7320508079979));
#6096=CARTESIAN_POINT('Ctrl Pts',(-1.41410031865014E-16,61.325000000286,
-2.30940107733053));
#6097=CARTESIAN_POINT('Ctrl Pts',(1.0000000002477,61.2666666669527,-1.7320508079979));
#6098=CARTESIAN_POINT('Ctrl Pts',(2.00000000049539,61.2083333336194,-1.15470053866527));
#6099=CARTESIAN_POINT('Ctrl Pts',(2.00000000049539,61.150000000286,-2.44929359890139E-16));
#6100=CARTESIAN_POINT('Ctrl Pts',(2.00000000049539,61.0916666669527,1.15470053866527));
#6101=CARTESIAN_POINT('Ctrl Pts',(1.0000000002477,61.0333333336194,1.7320508079979));
#6102=CARTESIAN_POINT('Ctrl Pts',(4.24230095595043E-16,60.975000000286,
2.30940107733053));
#6103=CARTESIAN_POINT('Ctrl Pts',(-1.0000000002477,60.9166666669527,1.7320508079979));
#6104=CARTESIAN_POINT('Ctrl Pts',(-2.00000000049539,60.8583333336194,1.15470053866527));
#6105=CARTESIAN_POINT('Ctrl Pts',(-2.00000000049539,60.800000000286,0.));
#6106=CARTESIAN_POINT('Ctrl Pts',(-2.00000000049539,60.7416666669527,-1.15470053866527));
#6107=CARTESIAN_POINT('Ctrl Pts',(-1.0000000002477,60.6833333336194,-1.7320508079979));
#6108=CARTESIAN_POINT('Ctrl Pts',(-1.41410031865014E-16,60.625000000286,
-2.30940107733053));
#6109=CARTESIAN_POINT('Ctrl Pts',(1.0000000002477,60.5666666669527,-1.7320508079979));
#6110=CARTESIAN_POINT('Ctrl Pts',(2.00000000049539,60.5083333336194,-1.15470053866527));
#6111=CARTESIAN_POINT('Ctrl Pts',(2.00000000049539,60.450000000286,-2.44929359890139E-16));
#6112=CARTESIAN_POINT('Ctrl Pts',(2.00000000049539,60.3916666669527,1.15470053866527));
#6113=CARTESIAN_POINT('Ctrl Pts',(1.0000000002477,60.3333333336194,1.7320508079979));
#6114=CARTESIAN_POINT('Ctrl Pts',(4.24230095595043E-16,60.275000000286,
2.30940107733053));
#6115=CARTESIAN_POINT('Ctrl Pts',(-1.0000000002477,60.2166666669527,1.7320508079979));
#6116=CARTESIAN_POINT('Ctrl Pts',(-2.00000000049539,60.1583333336194,1.15470053866527));
#6117=CARTESIAN_POINT('Ctrl Pts',(-2.00000000049539,60.100000000286,0.));
#6118=CARTESIAN_POINT('Ctrl Pts',(-2.00000000049539,60.0416666669527,-1.15470053866527));
#6119=CARTESIAN_POINT('Ctrl Pts',(-1.0000000002477,59.9833333336194,-1.7320508079979));
#6120=CARTESIAN_POINT('Ctrl Pts',(-1.41410031865014E-16,59.925000000286,
-2.30940107733053));
#6121=CARTESIAN_POINT('Ctrl Pts',(1.0000000002477,59.8666666669527,-1.7320508079979));
#6122=CARTESIAN_POINT('Ctrl Pts',(2.00000000049539,59.8083333336194,-1.15470053866527));
#6123=CARTESIAN_POINT('Ctrl Pts',(2.00000000049539,59.750000000286,-2.44929359890139E-16));
#6124=CARTESIAN_POINT('Ctrl Pts',(2.00000000049539,59.6916666669527,1.15470053866527));
#6125=CARTESIAN_POINT('Ctrl Pts',(1.0000000002477,59.6333333336194,1.7320508079979));
#6126=CARTESIAN_POINT('Ctrl Pts',(4.24230095595043E-16,59.575000000286,
2.30940107733053));
#6127=CARTESIAN_POINT('Ctrl Pts',(-1.0000000002477,59.5166666669527,1.7320508079979));
#6128=CARTESIAN_POINT('Ctrl Pts',(-2.00000000049539,59.4583333336194,1.15470053866527));
#6129=CARTESIAN_POINT('Ctrl Pts',(-2.00000000049539,59.400000000286,0.));
#6130=CARTESIAN_POINT('Ctrl Pts',(-2.00000000049539,59.3416666669527,-1.15470053866527));
#6131=CARTESIAN_POINT('Ctrl Pts',(-1.0000000002477,59.2833333336194,-1.7320508079979));
#6132=CARTESIAN_POINT('Ctrl Pts',(-1.41410031865014E-16,59.225000000286,
-2.30940107733053));
#6133=CARTESIAN_POINT('Ctrl Pts',(1.0000000002477,59.1666666669527,-1.7320508079979));
#6134=CARTESIAN_POINT('Ctrl Pts',(2.00000000049539,59.1083333336194,-1.15470053866527));
#6135=CARTESIAN_POINT('Ctrl Pts',(2.00000000049539,59.050000000286,-2.44929359890139E-16));
#6136=CARTESIAN_POINT('Ctrl Pts',(2.00000000049539,58.9916666669527,1.15470053866527));
#6137=CARTESIAN_POINT('Ctrl Pts',(1.0000000002477,58.9333333336194,1.7320508079979));
#6138=CARTESIAN_POINT('Ctrl Pts',(4.24230095595043E-16,58.875000000286,
2.30940107733053));
#6139=CARTESIAN_POINT('Ctrl Pts',(-1.0000000002477,58.8166666669527,1.7320508079979));
#6140=CARTESIAN_POINT('Ctrl Pts',(-2.00000000049539,58.7583333336194,1.15470053866527));
#6141=CARTESIAN_POINT('Ctrl Pts',(-2.00000000049539,58.700000000286,0.));
#6142=CARTESIAN_POINT('Ctrl Pts',(-2.00000000049539,58.6416666669527,-1.15470053866527));
#6143=CARTESIAN_POINT('Ctrl Pts',(-1.0000000002477,58.5833333336194,-1.7320508079979));
#6144=CARTESIAN_POINT('Ctrl Pts',(-1.41410031865014E-16,58.525000000286,
-2.30940107733053));
#6145=CARTESIAN_POINT('Ctrl Pts',(1.0000000002477,58.4666666669527,-1.7320508079979));
#6146=CARTESIAN_POINT('Ctrl Pts',(2.00000000049539,58.4083333336194,-1.15470053866527));
#6147=CARTESIAN_POINT('Ctrl Pts',(2.00000000049539,58.350000000286,-2.44929359890139E-16));
#6148=CARTESIAN_POINT('Ctrl Pts',(2.00000000049539,58.2916666669527,1.15470053866527));
#6149=CARTESIAN_POINT('Ctrl Pts',(1.0000000002477,58.2333333336194,1.7320508079979));
#6150=CARTESIAN_POINT('Ctrl Pts',(4.24230095595043E-16,58.175000000286,
2.30940107733053));
#6151=CARTESIAN_POINT('Ctrl Pts',(-1.0000000002477,58.1166666669527,1.7320508079979));
#6152=CARTESIAN_POINT('Ctrl Pts',(-2.00000000049539,58.0583333336194,1.15470053866527));
#6153=CARTESIAN_POINT('Ctrl Pts',(-2.00000000049539,58.000000000286,0.));
#6154=CARTESIAN_POINT('Ctrl Pts',(-2.00000000049539,57.9416666669527,-1.15470053866527));
#6155=CARTESIAN_POINT('Ctrl Pts',(-1.0000000002477,57.8833333336193,-1.7320508079979));
#6156=CARTESIAN_POINT('Ctrl Pts',(-1.41410031865014E-16,57.825000000286,
-2.30940107733053));
#6157=CARTESIAN_POINT('Ctrl Pts',(1.0000000002477,57.7666666669527,-1.7320508079979));
#6158=CARTESIAN_POINT('Ctrl Pts',(2.00000000049539,57.7083333336194,-1.15470053866527));
#6159=CARTESIAN_POINT('Ctrl Pts',(2.00000000049539,57.650000000286,-2.44929359890139E-16));
#6160=CARTESIAN_POINT('Ctrl Pts',(2.00000000049539,57.5916666669527,1.15470053866527));
#6161=CARTESIAN_POINT('Ctrl Pts',(1.0000000002477,57.5333333336194,1.7320508079979));
#6162=CARTESIAN_POINT('Ctrl Pts',(4.24230095595043E-16,57.475000000286,
2.30940107733053));
#6163=CARTESIAN_POINT('Ctrl Pts',(-1.0000000002477,57.4166666669527,1.7320508079979));
#6164=CARTESIAN_POINT('Ctrl Pts',(-2.00000000049539,57.3583333336194,1.15470053866527));
#6165=CARTESIAN_POINT('Ctrl Pts',(-2.00000000049539,57.300000000286,0.));
#6166=CARTESIAN_POINT('Ctrl Pts',(-2.00000000049539,57.2416666669527,-1.15470053866527));
#6167=CARTESIAN_POINT('Ctrl Pts',(-1.0000000002477,57.1833333336194,-1.7320508079979));
#6168=CARTESIAN_POINT('Ctrl Pts',(-1.41410031865014E-16,57.125000000286,
-2.30940107733053));
#6169=CARTESIAN_POINT('Ctrl Pts',(1.0000000002477,57.0666666669527,-1.7320508079979));
#6170=CARTESIAN_POINT('Ctrl Pts',(2.00000000049539,57.0083333336194,-1.15470053866527));
#6171=CARTESIAN_POINT('Ctrl Pts',(2.00000000049539,56.950000000286,-2.44929359890139E-16));
#6172=CARTESIAN_POINT('Ctrl Pts',(2.00000000049539,56.8916666669527,1.15470053866527));
#6173=CARTESIAN_POINT('Ctrl Pts',(1.0000000002477,56.8333333336194,1.7320508079979));
#6174=CARTESIAN_POINT('Ctrl Pts',(4.24230095595043E-16,56.775000000286,
2.30940107733053));
#6175=CARTESIAN_POINT('Ctrl Pts',(-1.0000000002477,56.7166666669527,1.7320508079979));
#6176=CARTESIAN_POINT('Ctrl Pts',(-2.00000000049539,56.6583333336194,1.15470053866527));
#6177=CARTESIAN_POINT('Ctrl Pts',(-2.00000000049539,56.600000000286,0.));
#6178=CARTESIAN_POINT('Ctrl Pts',(-2.00000000049539,56.5416666669527,-1.15470053866527));
#6179=CARTESIAN_POINT('Ctrl Pts',(-1.0000000002477,56.4833333336194,-1.7320508079979));
#6180=CARTESIAN_POINT('Ctrl Pts',(-1.41410031865014E-16,56.425000000286,
-2.30940107733053));
#6181=CARTESIAN_POINT('Ctrl Pts',(1.0000000002477,56.3666666669527,-1.7320508079979));
#6182=CARTESIAN_POINT('Ctrl Pts',(2.00000000049539,56.3083333336194,-1.15470053866527));
#6183=CARTESIAN_POINT('Ctrl Pts',(2.00000000049539,56.250000000286,-2.44929359890139E-16));
#6184=CARTESIAN_POINT('Ctrl Pts',(2.00000000049539,56.1916666669527,1.15470053866527));
#6185=CARTESIAN_POINT('Ctrl Pts',(1.0000000002477,56.1333333336194,1.7320508079979));
#6186=CARTESIAN_POINT('Ctrl Pts',(4.24230095595043E-16,56.075000000286,
2.30940107733053));
#6187=CARTESIAN_POINT('Ctrl Pts',(-1.0000000002477,56.0166666669527,1.7320508079979));
#6188=CARTESIAN_POINT('Ctrl Pts',(-2.00000000049539,55.9583333336194,1.15470053866527));
#6189=CARTESIAN_POINT('Ctrl Pts',(-2.00000000049539,55.900000000286,0.));
#6190=CARTESIAN_POINT('Ctrl Pts',(-2.00000000049539,55.8416666669527,-1.15470053866527));
#6191=CARTESIAN_POINT('Ctrl Pts',(-1.0000000002477,55.7833333336194,-1.7320508079979));
#6192=CARTESIAN_POINT('Ctrl Pts',(-1.41410031865014E-16,55.725000000286,
-2.30940107733053));
#6193=CARTESIAN_POINT('Ctrl Pts',(1.0000000002477,55.6666666669527,-1.7320508079979));
#6194=CARTESIAN_POINT('Ctrl Pts',(2.00000000049539,55.6083333336194,-1.15470053866527));
#6195=CARTESIAN_POINT('Ctrl Pts',(2.00000000049539,55.550000000286,-2.44929359890139E-16));
#6196=CARTESIAN_POINT('Ctrl Pts',(2.00000000049539,55.4916666669527,1.15470053866527));
#6197=CARTESIAN_POINT('Ctrl Pts',(1.0000000002477,55.4333333336194,1.7320508079979));
#6198=CARTESIAN_POINT('Ctrl Pts',(4.24230095595043E-16,55.375000000286,
2.30940107733053));
#6199=CARTESIAN_POINT('Ctrl Pts',(-1.0000000002477,55.3166666669527,1.7320508079979));
#6200=CARTESIAN_POINT('Ctrl Pts',(-2.00000000049539,55.2583333336194,1.15470053866527));
#6201=CARTESIAN_POINT('Ctrl Pts',(-2.00000000049539,55.200000000286,0.));
#6202=CARTESIAN_POINT('Ctrl Pts',(-2.00000000049539,55.1416666669527,-1.15470053866527));
#6203=CARTESIAN_POINT('Ctrl Pts',(-1.0000000002477,55.0833333336194,-1.7320508079979));
#6204=CARTESIAN_POINT('Ctrl Pts',(-1.41410031865014E-16,55.025000000286,
-2.30940107733053));
#6205=CARTESIAN_POINT('Ctrl Pts',(1.0000000002477,54.9666666669527,-1.7320508079979));
#6206=CARTESIAN_POINT('Ctrl Pts',(2.00000000049539,54.9083333336194,-1.15470053866527));
#6207=CARTESIAN_POINT('Ctrl Pts',(2.00000000049539,54.850000000286,-2.44929359890139E-16));
#6208=CARTESIAN_POINT('Ctrl Pts',(2.00000000049539,54.7916666669527,1.15470053866527));
#6209=CARTESIAN_POINT('Ctrl Pts',(1.0000000002477,54.7333333336194,1.7320508079979));
#6210=CARTESIAN_POINT('Ctrl Pts',(4.24230095595043E-16,54.675000000286,
2.30940107733053));
#6211=CARTESIAN_POINT('Ctrl Pts',(-1.0000000002477,54.6166666669527,1.7320508079979));
#6212=CARTESIAN_POINT('Ctrl Pts',(-2.00000000049539,54.5583333336194,1.15470053866527));
#6213=CARTESIAN_POINT('Ctrl Pts',(-2.00000000049539,54.500000000286,0.));
#6214=CARTESIAN_POINT('Ctrl Pts',(-2.00000000049539,54.4416666669527,-1.15470053866527));
#6215=CARTESIAN_POINT('Ctrl Pts',(-1.0000000002477,54.3833333336194,-1.7320508079979));
#6216=CARTESIAN_POINT('Ctrl Pts',(-1.41410031865014E-16,54.325000000286,
-2.30940107733053));
#6217=CARTESIAN_POINT('Ctrl Pts',(1.0000000002477,54.2666666669527,-1.7320508079979));
#6218=CARTESIAN_POINT('Ctrl Pts',(2.00000000049539,54.2083333336194,-1.15470053866527));
#6219=CARTESIAN_POINT('Ctrl Pts',(2.00000000049539,54.150000000286,-2.44929359890139E-16));
#6220=CARTESIAN_POINT('Ctrl Pts',(2.00000000049539,54.0916666669527,1.15470053866527));
#6221=CARTESIAN_POINT('Ctrl Pts',(1.0000000002477,54.0333333336194,1.7320508079979));
#6222=CARTESIAN_POINT('Ctrl Pts',(4.24230095595043E-16,53.975000000286,
2.30940107733053));
#6223=CARTESIAN_POINT('Ctrl Pts',(-1.0000000002477,53.9166666669527,1.7320508079979));
#6224=CARTESIAN_POINT('Ctrl Pts',(-2.00000000049539,53.8583333336194,1.15470053866527));
#6225=CARTESIAN_POINT('Ctrl Pts',(-2.00000000049539,53.800000000286,0.));
#6226=CARTESIAN_POINT('Ctrl Pts',(-2.00000000049539,53.7416666669527,-1.15470053866527));
#6227=CARTESIAN_POINT('Ctrl Pts',(-1.0000000002477,53.6833333336194,-1.7320508079979));
#6228=CARTESIAN_POINT('Ctrl Pts',(-1.41410031865014E-16,53.625000000286,
-2.30940107733053));
#6229=CARTESIAN_POINT('Ctrl Pts',(1.0000000002477,53.5666666669527,-1.7320508079979));
#6230=CARTESIAN_POINT('Ctrl Pts',(2.00000000049539,53.5083333336194,-1.15470053866527));
#6231=CARTESIAN_POINT('Ctrl Pts',(2.00000000049539,53.450000000286,-2.44929359890139E-16));
#6232=CARTESIAN_POINT('Ctrl Pts',(2.00000000049539,53.3916666669527,1.15470053866527));
#6233=CARTESIAN_POINT('Ctrl Pts',(1.0000000002477,53.3333333336194,1.7320508079979));
#6234=CARTESIAN_POINT('Ctrl Pts',(4.24230095595043E-16,53.275000000286,
2.30940107733053));
#6235=CARTESIAN_POINT('Ctrl Pts',(-1.0000000002477,53.2166666669527,1.7320508079979));
#6236=CARTESIAN_POINT('Ctrl Pts',(-2.00000000049539,53.1583333336194,1.15470053866527));
#6237=CARTESIAN_POINT('Ctrl Pts',(-2.00000000049539,53.100000000286,0.));
#6238=CARTESIAN_POINT('Ctrl Pts',(-2.00000000049539,53.0416666669527,-1.15470053866527));
#6239=CARTESIAN_POINT('Ctrl Pts',(-1.0000000002477,52.9833333336194,-1.7320508079979));
#6240=CARTESIAN_POINT('Ctrl Pts',(-1.41410031865014E-16,52.925000000286,
-2.30940107733053));
#6241=CARTESIAN_POINT('Ctrl Pts',(1.0000000002477,52.8666666669527,-1.7320508079979));
#6242=CARTESIAN_POINT('Ctrl Pts',(2.00000000049539,52.8083333336193,-1.15470053866527));
#6243=CARTESIAN_POINT('Ctrl Pts',(2.00000000049539,52.750000000286,-2.44929359890139E-16));
#6244=CARTESIAN_POINT('Ctrl Pts',(2.00000000049539,52.6916666669527,1.15470053866527));
#6245=CARTESIAN_POINT('Ctrl Pts',(1.0000000002477,52.6333333336194,1.7320508079979));
#6246=CARTESIAN_POINT('Ctrl Pts',(4.24230095595043E-16,52.575000000286,
2.30940107733053));
#6247=CARTESIAN_POINT('Ctrl Pts',(-1.0000000002477,52.5166666669527,1.7320508079979));
#6248=CARTESIAN_POINT('Ctrl Pts',(-2.00000000049539,52.4583333336194,1.15470053866527));
#6249=CARTESIAN_POINT('Ctrl Pts',(-2.00000000049539,52.400000000286,0.));
#6250=CARTESIAN_POINT('Ctrl Pts',(-2.00000000049539,52.3416666669527,-1.15470053866527));
#6251=CARTESIAN_POINT('Ctrl Pts',(-1.0000000002477,52.2833333336194,-1.7320508079979));
#6252=CARTESIAN_POINT('Ctrl Pts',(-1.41410031865014E-16,52.225000000286,
-2.30940107733053));
#6253=CARTESIAN_POINT('Ctrl Pts',(1.0000000002477,52.1666666669527,-1.7320508079979));
#6254=CARTESIAN_POINT('Ctrl Pts',(2.00000000049539,52.1083333336194,-1.15470053866527));
#6255=CARTESIAN_POINT('Ctrl Pts',(2.00000000049539,52.050000000286,-2.44929359890139E-16));
#6256=CARTESIAN_POINT('Ctrl Pts',(2.00000000049539,51.9916666669527,1.15470053866527));
#6257=CARTESIAN_POINT('Ctrl Pts',(1.0000000002477,51.9333333336194,1.7320508079979));
#6258=CARTESIAN_POINT('Ctrl Pts',(4.24230095595043E-16,51.875000000286,
2.30940107733053));
#6259=CARTESIAN_POINT('Ctrl Pts',(-1.0000000002477,51.8166666669527,1.7320508079979));
#6260=CARTESIAN_POINT('Ctrl Pts',(-2.00000000049539,51.7583333336194,1.15470053866527));
#6261=CARTESIAN_POINT('Ctrl Pts',(-2.00000000049539,51.700000000286,0.));
#6262=CARTESIAN_POINT('Ctrl Pts',(-2.00000000049539,51.6416666669527,-1.15470053866527));
#6263=CARTESIAN_POINT('Ctrl Pts',(-1.0000000002477,51.5833333336194,-1.7320508079979));
#6264=CARTESIAN_POINT('Ctrl Pts',(-1.41410031865014E-16,51.525000000286,
-2.30940107733053));
#6265=CARTESIAN_POINT('Ctrl Pts',(1.0000000002477,51.4666666669527,-1.7320508079979));
#6266=CARTESIAN_POINT('Ctrl Pts',(2.00000000049539,51.4083333336194,-1.15470053866527));
#6267=CARTESIAN_POINT('Ctrl Pts',(2.00000000049539,51.350000000286,-2.44929359890139E-16));
#6268=CARTESIAN_POINT('Ctrl Pts',(2.00000000049539,51.2916666669527,1.15470053866527));
#6269=CARTESIAN_POINT('Ctrl Pts',(1.0000000002477,51.2333333336194,1.7320508079979));
#6270=CARTESIAN_POINT('Ctrl Pts',(4.24230095595043E-16,51.175000000286,
2.30940107733053));
#6271=CARTESIAN_POINT('Ctrl Pts',(-1.0000000002477,51.1166666669527,1.7320508079979));
#6272=CARTESIAN_POINT('Ctrl Pts',(-2.00000000049539,51.0583333336194,1.15470053866527));
#6273=CARTESIAN_POINT('Ctrl Pts',(-2.00000000049539,51.000000000286,0.));
#6274=CARTESIAN_POINT('Ctrl Pts',(-2.00000000049539,50.9416666669527,-1.15470053866527));
#6275=CARTESIAN_POINT('Ctrl Pts',(-1.0000000002477,50.8833333336194,-1.7320508079979));
#6276=CARTESIAN_POINT('Ctrl Pts',(-1.41410031865014E-16,50.825000000286,
-2.30940107733053));
#6277=CARTESIAN_POINT('Ctrl Pts',(1.0000000002477,50.7666666669527,-1.7320508079979));
#6278=CARTESIAN_POINT('Ctrl Pts',(2.00000000049539,50.7083333336194,-1.15470053866527));
#6279=CARTESIAN_POINT('Ctrl Pts',(2.00000000049539,50.650000000286,-2.44929359890139E-16));
#6280=CARTESIAN_POINT('Ctrl Pts',(2.00000000049539,50.5916666669527,1.15470053866527));
#6281=CARTESIAN_POINT('Ctrl Pts',(1.0000000002477,50.5333333336194,1.7320508079979));
#6282=CARTESIAN_POINT('Ctrl Pts',(4.24230095595043E-16,50.475000000286,
2.30940107733053));
#6283=CARTESIAN_POINT('Ctrl Pts',(-1.0000000002477,50.4166666669527,1.7320508079979));
#6284=CARTESIAN_POINT('Ctrl Pts',(-2.00000000049539,50.3583333336194,1.15470053866527));
#6285=CARTESIAN_POINT('Ctrl Pts',(-2.00000000049539,50.300000000286,0.));
#6286=CARTESIAN_POINT('Ctrl Pts',(-2.00000000049539,50.2416666669527,-1.15470053866527));
#6287=CARTESIAN_POINT('Ctrl Pts',(-1.0000000002477,50.1833333336194,-1.7320508079979));
#6288=CARTESIAN_POINT('Ctrl Pts',(-1.41410031865014E-16,50.125000000286,
-2.30940107733053));
#6289=CARTESIAN_POINT('Ctrl Pts',(1.0000000002477,50.0666666669527,-1.7320508079979));
#6290=CARTESIAN_POINT('Ctrl Pts',(2.00000000049539,50.0083333336194,-1.15470053866527));
#6291=CARTESIAN_POINT('Ctrl Pts',(2.00000000049539,49.950000000286,-2.44929359890139E-16));
#6292=CARTESIAN_POINT('Ctrl Pts',(2.00000000049539,49.8916666669527,1.15470053866527));
#6293=CARTESIAN_POINT('Ctrl Pts',(1.0000000002477,49.8333333336194,1.7320508079979));
#6294=CARTESIAN_POINT('Ctrl Pts',(4.24230095595043E-16,49.775000000286,
2.30940107733053));
#6295=CARTESIAN_POINT('Ctrl Pts',(-1.0000000002477,49.7166666669527,1.7320508079979));
#6296=CARTESIAN_POINT('Ctrl Pts',(-2.00000000049539,49.6583333336194,1.15470053866527));
#6297=CARTESIAN_POINT('Ctrl Pts',(-2.00000000049539,49.600000000286,0.));
#6298=CARTESIAN_POINT('Ctrl Pts',(-2.00000000049539,49.5416666669527,-1.15470053866527));
#6299=CARTESIAN_POINT('Ctrl Pts',(-1.0000000002477,49.4833333336194,-1.7320508079979));
#6300=CARTESIAN_POINT('Ctrl Pts',(-1.41410031865014E-16,49.425000000286,
-2.30940107733053));
#6301=CARTESIAN_POINT('Ctrl Pts',(1.0000000002477,49.3666666669527,-1.7320508079979));
#6302=CARTESIAN_POINT('Ctrl Pts',(2.00000000049539,49.3083333336194,-1.15470053866527));
#6303=CARTESIAN_POINT('Ctrl Pts',(2.00000000049539,49.250000000286,-2.44929359890139E-16));
#6304=CARTESIAN_POINT('Ctrl Pts',(2.00000000049539,49.1916666669527,1.15470053866527));
#6305=CARTESIAN_POINT('Ctrl Pts',(1.0000000002477,49.1333333336194,1.7320508079979));
#6306=CARTESIAN_POINT('Ctrl Pts',(4.24230095595043E-16,49.075000000286,
2.30940107733053));
#6307=CARTESIAN_POINT('Ctrl Pts',(-1.0000000002477,49.0166666669527,1.7320508079979));
#6308=CARTESIAN_POINT('Ctrl Pts',(-2.00000000049539,48.9583333336194,1.15470053866527));
#6309=CARTESIAN_POINT('Ctrl Pts',(-2.00000000049539,48.900000000286,0.));
#6310=CARTESIAN_POINT('Ctrl Pts',(-2.00000000049539,48.8416666669527,-1.15470053866527));
#6311=CARTESIAN_POINT('Ctrl Pts',(-1.0000000002477,48.7833333336194,-1.7320508079979));
#6312=CARTESIAN_POINT('Ctrl Pts',(-1.41410031865014E-16,48.725000000286,
-2.30940107733053));
#6313=CARTESIAN_POINT('Ctrl Pts',(1.0000000002477,48.6666666669527,-1.7320508079979));
#6314=CARTESIAN_POINT('Ctrl Pts',(2.00000000049539,48.6083333336194,-1.15470053866527));
#6315=CARTESIAN_POINT('Ctrl Pts',(2.00000000049539,48.550000000286,-2.44929359890139E-16));
#6316=CARTESIAN_POINT('Ctrl Pts',(2.00000000049539,48.4916666669527,1.15470053866527));
#6317=CARTESIAN_POINT('Ctrl Pts',(1.0000000002477,48.4333333336194,1.7320508079979));
#6318=CARTESIAN_POINT('Ctrl Pts',(4.24230095595043E-16,48.375000000286,
2.30940107733053));
#6319=CARTESIAN_POINT('Ctrl Pts',(-1.0000000002477,48.3166666669527,1.7320508079979));
#6320=CARTESIAN_POINT('Ctrl Pts',(-2.00000000049539,48.2583333336193,1.15470053866527));
#6321=CARTESIAN_POINT('Ctrl Pts',(-2.00000000049539,48.200000000286,0.));
#6322=CARTESIAN_POINT('Ctrl Pts',(-2.00000000049539,48.1416666669527,-1.15470053866527));
#6323=CARTESIAN_POINT('Ctrl Pts',(-1.0000000002477,48.0833333336194,-1.7320508079979));
#6324=CARTESIAN_POINT('Ctrl Pts',(-1.41410031865014E-16,48.025000000286,
-2.30940107733053));
#6325=CARTESIAN_POINT('Ctrl Pts',(1.0000000002477,47.9666666669527,-1.7320508079979));
#6326=CARTESIAN_POINT('Ctrl Pts',(2.00000000049539,47.9083333336194,-1.15470053866527));
#6327=CARTESIAN_POINT('Ctrl Pts',(2.00000000049539,47.850000000286,-2.44929359890139E-16));
#6328=CARTESIAN_POINT('Ctrl Pts',(2.00000000049539,47.7916666669527,1.15470053866527));
#6329=CARTESIAN_POINT('Ctrl Pts',(1.0000000002477,47.7333333336194,1.7320508079979));
#6330=CARTESIAN_POINT('Ctrl Pts',(4.24230095595043E-16,47.675000000286,
2.30940107733053));
#6331=CARTESIAN_POINT('Ctrl Pts',(-1.0000000002477,47.6166666669527,1.7320508079979));
#6332=CARTESIAN_POINT('Ctrl Pts',(-2.00000000049539,47.5583333336194,1.15470053866527));
#6333=CARTESIAN_POINT('Ctrl Pts',(-2.00000000049539,47.500000000286,0.));
#6334=CARTESIAN_POINT('Ctrl Pts',(-2.00000000049539,47.4416666669527,-1.15470053866527));
#6335=CARTESIAN_POINT('Ctrl Pts',(-1.0000000002477,47.3833333336194,-1.7320508079979));
#6336=CARTESIAN_POINT('Ctrl Pts',(-1.41410031865014E-16,47.325000000286,
-2.30940107733053));
#6337=CARTESIAN_POINT('Ctrl Pts',(1.0000000002477,47.2666666669527,-1.7320508079979));
#6338=CARTESIAN_POINT('Ctrl Pts',(2.00000000049539,47.2083333336194,-1.15470053866527));
#6339=CARTESIAN_POINT('Ctrl Pts',(2.00000000049539,47.150000000286,-2.44929359890139E-16));
#6340=CARTESIAN_POINT('Ctrl Pts',(2.00000000049539,47.0916666669527,1.15470053866527));
#6341=CARTESIAN_POINT('Ctrl Pts',(1.0000000002477,47.0333333336194,1.7320508079979));
#6342=CARTESIAN_POINT('Ctrl Pts',(4.24230095595043E-16,46.975000000286,
2.30940107733053));
#6343=CARTESIAN_POINT('Ctrl Pts',(-1.0000000002477,46.9166666669527,1.7320508079979));
#6344=CARTESIAN_POINT('Ctrl Pts',(-2.00000000049539,46.8583333336193,1.15470053866527));
#6345=CARTESIAN_POINT('Ctrl Pts',(-2.00000000049539,46.800000000286,0.));
#6346=CARTESIAN_POINT('Ctrl Pts',(-2.00000000049539,46.7416666669527,-1.15470053866527));
#6347=CARTESIAN_POINT('Ctrl Pts',(-1.0000000002477,46.6833333336194,-1.7320508079979));
#6348=CARTESIAN_POINT('Ctrl Pts',(-1.41410031865014E-16,46.625000000286,
-2.30940107733053));
#6349=CARTESIAN_POINT('Ctrl Pts',(1.0000000002477,46.5666666669527,-1.7320508079979));
#6350=CARTESIAN_POINT('Ctrl Pts',(2.00000000049539,46.5083333336194,-1.15470053866527));
#6351=CARTESIAN_POINT('Ctrl Pts',(2.00000000049539,46.450000000286,-2.44929359890139E-16));
#6352=CARTESIAN_POINT('Ctrl Pts',(2.00000000049539,46.3916666669527,1.15470053866527));
#6353=CARTESIAN_POINT('Ctrl Pts',(1.0000000002477,46.3333333336194,1.7320508079979));
#6354=CARTESIAN_POINT('Ctrl Pts',(4.24230095595043E-16,46.275000000286,
2.30940107733053));
#6355=CARTESIAN_POINT('Ctrl Pts',(-1.0000000002477,46.2166666669527,1.7320508079979));
#6356=CARTESIAN_POINT('Ctrl Pts',(-2.00000000049539,46.1583333336193,1.15470053866527));
#6357=CARTESIAN_POINT('Ctrl Pts',(-2.00000000049539,46.100000000286,0.));
#6358=CARTESIAN_POINT('Ctrl Pts',(-2.00000000049539,46.0416666669527,-1.15470053866527));
#6359=CARTESIAN_POINT('Ctrl Pts',(-1.0000000002477,45.9833333336194,-1.7320508079979));
#6360=CARTESIAN_POINT('Ctrl Pts',(-1.41410031865014E-16,45.925000000286,
-2.30940107733053));
#6361=CARTESIAN_POINT('Ctrl Pts',(1.0000000002477,45.8666666669527,-1.7320508079979));
#6362=CARTESIAN_POINT('Ctrl Pts',(2.00000000049539,45.8083333336194,-1.15470053866527));
#6363=CARTESIAN_POINT('Ctrl Pts',(2.00000000049539,45.750000000286,-2.44929359890139E-16));
#6364=CARTESIAN_POINT('Ctrl Pts',(2.00000000049539,45.6916666669527,1.15470053866527));
#6365=CARTESIAN_POINT('Ctrl Pts',(1.0000000002477,45.6333333336194,1.7320508079979));
#6366=CARTESIAN_POINT('Ctrl Pts',(4.24230095595043E-16,45.575000000286,
2.30940107733053));
#6367=CARTESIAN_POINT('Ctrl Pts',(-1.0000000002477,45.5166666669527,1.7320508079979));
#6368=CARTESIAN_POINT('Ctrl Pts',(-2.00000000049539,45.4583333336194,1.15470053866527));
#6369=CARTESIAN_POINT('Ctrl Pts',(-2.00000000049539,45.400000000286,0.));
#6370=CARTESIAN_POINT('Ctrl Pts',(-2.00000000049539,45.3416666669527,-1.15470053866527));
#6371=CARTESIAN_POINT('Ctrl Pts',(-1.0000000002477,45.2833333336194,-1.7320508079979));
#6372=CARTESIAN_POINT('Ctrl Pts',(-1.41410031865014E-16,45.225000000286,
-2.30940107733053));
#6373=CARTESIAN_POINT('Ctrl Pts',(1.0000000002477,45.1666666669527,-1.7320508079979));
#6374=CARTESIAN_POINT('Ctrl Pts',(2.00000000049539,45.1083333336194,-1.15470053866527));
#6375=CARTESIAN_POINT('Ctrl Pts',(2.00000000049539,45.050000000286,-2.44929359890139E-16));
#6376=CARTESIAN_POINT('Ctrl Pts',(2.00000000049539,44.9916666669527,1.15470053866527));
#6377=CARTESIAN_POINT('Ctrl Pts',(1.0000000002477,44.9333333336194,1.7320508079979));
#6378=CARTESIAN_POINT('Ctrl Pts',(4.24230095595043E-16,44.875000000286,
2.30940107733053));
#6379=CARTESIAN_POINT('Ctrl Pts',(-1.0000000002477,44.8166666669527,1.7320508079979));
#6380=CARTESIAN_POINT('Ctrl Pts',(-2.00000000049539,44.7583333336194,1.15470053866527));
#6381=CARTESIAN_POINT('Ctrl Pts',(-2.00000000049539,44.700000000286,0.));
#6382=CARTESIAN_POINT('Ctrl Pts',(-2.00000000049539,44.6416666669527,-1.15470053866527));
#6383=CARTESIAN_POINT('Ctrl Pts',(-1.0000000002477,44.5833333336194,-1.7320508079979));
#6384=CARTESIAN_POINT('Ctrl Pts',(-1.41410031865014E-16,44.525000000286,
-2.30940107733053));
#6385=CARTESIAN_POINT('Ctrl Pts',(1.0000000002477,44.4666666669527,-1.7320508079979));
#6386=CARTESIAN_POINT('Ctrl Pts',(2.00000000049539,44.4083333336194,-1.15470053866527));
#6387=CARTESIAN_POINT('Ctrl Pts',(2.00000000049539,44.350000000286,-2.44929359890139E-16));
#6388=CARTESIAN_POINT('Ctrl Pts',(2.00000000049539,44.2916666669527,1.15470053866527));
#6389=CARTESIAN_POINT('Ctrl Pts',(1.0000000002477,44.2333333336194,1.7320508079979));
#6390=CARTESIAN_POINT('Ctrl Pts',(4.24230095595043E-16,44.175000000286,
2.30940107733053));
#6391=CARTESIAN_POINT('Ctrl Pts',(-1.0000000002477,44.1166666669527,1.7320508079979));
#6392=CARTESIAN_POINT('Ctrl Pts',(-2.00000000049539,44.0583333336194,1.15470053866527));
#6393=CARTESIAN_POINT('Ctrl Pts',(-2.00000000049539,44.000000000286,0.));
#6394=CARTESIAN_POINT('Ctrl Pts',(-2.00000000049539,43.9416666669527,-1.15470053866527));
#6395=CARTESIAN_POINT('Ctrl Pts',(-1.0000000002477,43.8833333336194,-1.7320508079979));
#6396=CARTESIAN_POINT('Ctrl Pts',(-1.41410031865014E-16,43.825000000286,
-2.30940107733053));
#6397=CARTESIAN_POINT('Ctrl Pts',(1.0000000002477,43.7666666669527,-1.7320508079979));
#6398=CARTESIAN_POINT('Ctrl Pts',(2.00000000049539,43.7083333336194,-1.15470053866527));
#6399=CARTESIAN_POINT('Ctrl Pts',(2.00000000049539,43.650000000286,-2.44929359890139E-16));
#6400=CARTESIAN_POINT('Ctrl Pts',(2.00000000049539,43.5916666669527,1.15470053866527));
#6401=CARTESIAN_POINT('Ctrl Pts',(1.0000000002477,43.5333333336194,1.7320508079979));
#6402=CARTESIAN_POINT('Ctrl Pts',(4.24230095595043E-16,43.475000000286,
2.30940107733053));
#6403=CARTESIAN_POINT('Ctrl Pts',(-1.0000000002477,43.4166666669527,1.7320508079979));
#6404=CARTESIAN_POINT('Ctrl Pts',(-2.00000000049539,43.3583333336194,1.15470053866527));
#6405=CARTESIAN_POINT('Ctrl Pts',(-2.00000000049539,43.300000000286,0.));
#6406=CARTESIAN_POINT('Ctrl Pts',(-2.00000000049539,43.2416666669527,-1.15470053866527));
#6407=CARTESIAN_POINT('Ctrl Pts',(-1.0000000002477,43.1833333336194,-1.7320508079979));
#6408=CARTESIAN_POINT('Ctrl Pts',(-1.41410031865014E-16,43.125000000286,
-2.30940107733053));
#6409=CARTESIAN_POINT('Ctrl Pts',(1.0000000002477,43.0666666669527,-1.7320508079979));
#6410=CARTESIAN_POINT('Ctrl Pts',(2.00000000049539,43.0083333336194,-1.15470053866527));
#6411=CARTESIAN_POINT('Ctrl Pts',(2.00000000049539,42.950000000286,-2.44929359890139E-16));
#6412=CARTESIAN_POINT('Ctrl Pts',(2.00000000049539,42.8916666669527,1.15470053866527));
#6413=CARTESIAN_POINT('Ctrl Pts',(1.0000000002477,42.8333333336194,1.7320508079979));
#6414=CARTESIAN_POINT('Ctrl Pts',(4.24230095595043E-16,42.775000000286,
2.30940107733053));
#6415=CARTESIAN_POINT('Ctrl Pts',(-1.0000000002477,42.7166666669527,1.7320508079979));
#6416=CARTESIAN_POINT('Ctrl Pts',(-2.00000000049539,42.6583333336194,1.15470053866527));
#6417=CARTESIAN_POINT('Ctrl Pts',(-2.00000000049539,42.600000000286,0.));
#6418=CARTESIAN_POINT('Ctrl Pts',(-2.00000000049539,42.5416666669527,-1.15470053866527));
#6419=CARTESIAN_POINT('Ctrl Pts',(-1.0000000002477,42.4833333336194,-1.7320508079979));
#6420=CARTESIAN_POINT('Ctrl Pts',(-1.41410031865014E-16,42.425000000286,
-2.30940107733053));
#6421=CARTESIAN_POINT('Ctrl Pts',(1.0000000002477,42.3666666669527,-1.7320508079979));
#6422=CARTESIAN_POINT('Ctrl Pts',(2.00000000049539,42.3083333336194,-1.15470053866527));
#6423=CARTESIAN_POINT('Ctrl Pts',(2.00000000049539,42.250000000286,-2.44929359890139E-16));
#6424=CARTESIAN_POINT('Ctrl Pts',(2.00000000049539,42.1916666669527,1.15470053866527));
#6425=CARTESIAN_POINT('Ctrl Pts',(1.0000000002477,42.1333333336194,1.7320508079979));
#6426=CARTESIAN_POINT('Ctrl Pts',(4.24230095595043E-16,42.075000000286,
2.30940107733053));
#6427=CARTESIAN_POINT('Ctrl Pts',(-1.0000000002477,42.0166666669527,1.7320508079979));
#6428=CARTESIAN_POINT('Ctrl Pts',(-2.00000000049539,41.9583333336194,1.15470053866527));
#6429=CARTESIAN_POINT('Ctrl Pts',(-2.00000000049539,41.900000000286,0.));
#6430=CARTESIAN_POINT('Ctrl Pts',(-2.00000000049539,41.8416666669527,-1.15470053866527));
#6431=CARTESIAN_POINT('Ctrl Pts',(-1.0000000002477,41.7833333336194,-1.7320508079979));
#6432=CARTESIAN_POINT('Ctrl Pts',(-1.41410031865014E-16,41.725000000286,
-2.30940107733053));
#6433=CARTESIAN_POINT('Ctrl Pts',(1.0000000002477,41.6666666669527,-1.7320508079979));
#6434=CARTESIAN_POINT('Ctrl Pts',(2.00000000049539,41.6083333336194,-1.15470053866527));
#6435=CARTESIAN_POINT('Ctrl Pts',(2.00000000049539,41.550000000286,-2.44929359890139E-16));
#6436=CARTESIAN_POINT('Ctrl Pts',(2.00000000049539,41.4916666669527,1.15470053866527));
#6437=CARTESIAN_POINT('Ctrl Pts',(1.0000000002477,41.4333333336194,1.7320508079979));
#6438=CARTESIAN_POINT('Ctrl Pts',(4.24230095595043E-16,41.375000000286,
2.30940107733053));
#6439=CARTESIAN_POINT('Ctrl Pts',(-1.0000000002477,41.3166666669527,1.7320508079979));
#6440=CARTESIAN_POINT('Ctrl Pts',(-2.00000000049539,41.2583333336194,1.15470053866527));
#6441=CARTESIAN_POINT('Ctrl Pts',(-2.00000000049539,41.200000000286,0.));
#6442=CARTESIAN_POINT('Ctrl Pts',(-2.00000000049539,41.1416666669527,-1.15470053866527));
#6443=CARTESIAN_POINT('Ctrl Pts',(-1.0000000002477,41.0833333336194,-1.7320508079979));
#6444=CARTESIAN_POINT('Ctrl Pts',(-1.41410031865014E-16,41.025000000286,
-2.30940107733053));
#6445=CARTESIAN_POINT('Ctrl Pts',(1.0000000002477,40.9666666669527,-1.7320508079979));
#6446=CARTESIAN_POINT('Ctrl Pts',(2.00000000049539,40.9083333336194,-1.15470053866527));
#6447=CARTESIAN_POINT('Ctrl Pts',(2.00000000049539,40.850000000286,-2.44929359890139E-16));
#6448=CARTESIAN_POINT('Ctrl Pts',(2.00000000049539,40.7916666669527,1.15470053866527));
#6449=CARTESIAN_POINT('Ctrl Pts',(1.0000000002477,40.7333333336194,1.7320508079979));
#6450=CARTESIAN_POINT('Ctrl Pts',(4.24230095595043E-16,40.675000000286,
2.30940107733053));
#6451=CARTESIAN_POINT('Ctrl Pts',(-1.0000000002477,40.6166666669527,1.7320508079979));
#6452=CARTESIAN_POINT('Ctrl Pts',(-2.00000000049539,40.5583333336194,1.15470053866527));
#6453=CARTESIAN_POINT('Ctrl Pts',(-2.00000000049539,40.500000000286,0.));
#6454=CARTESIAN_POINT('Ctrl Pts',(-2.00000000049539,40.4416666669527,-1.15470053866527));
#6455=CARTESIAN_POINT('Ctrl Pts',(-1.0000000002477,40.3833333336193,-1.7320508079979));
#6456=CARTESIAN_POINT('Ctrl Pts',(-1.41410031865014E-16,40.325000000286,
-2.30940107733053));
#6457=CARTESIAN_POINT('Ctrl Pts',(1.0000000002477,40.2666666669527,-1.7320508079979));
#6458=CARTESIAN_POINT('Ctrl Pts',(2.00000000049539,40.2083333336194,-1.15470053866527));
#6459=CARTESIAN_POINT('Ctrl Pts',(2.00000000049539,40.150000000286,-2.44929359890139E-16));
#6460=CARTESIAN_POINT('Ctrl Pts',(2.00000000049539,40.0916666669527,1.15470053866527));
#6461=CARTESIAN_POINT('Ctrl Pts',(1.0000000002477,40.0333333336194,1.7320508079979));
#6462=CARTESIAN_POINT('Ctrl Pts',(4.24230095595043E-16,39.975000000286,
2.30940107733053));
#6463=CARTESIAN_POINT('Ctrl Pts',(-1.0000000002477,39.9166666669527,1.7320508079979));
#6464=CARTESIAN_POINT('Ctrl Pts',(-2.00000000049539,39.8583333336194,1.15470053866527));
#6465=CARTESIAN_POINT('Ctrl Pts',(-2.00000000049539,39.800000000286,0.));
#6466=CARTESIAN_POINT('Ctrl Pts',(-2.00000000049539,39.7416666669527,-1.15470053866527));
#6467=CARTESIAN_POINT('Ctrl Pts',(-1.0000000002477,39.6833333336194,-1.7320508079979));
#6468=CARTESIAN_POINT('Ctrl Pts',(-1.41410031865014E-16,39.625000000286,
-2.30940107733053));
#6469=CARTESIAN_POINT('Ctrl Pts',(1.0000000002477,39.5666666669527,-1.7320508079979));
#6470=CARTESIAN_POINT('Ctrl Pts',(2.00000000049539,39.5083333336194,-1.15470053866527));
#6471=CARTESIAN_POINT('Ctrl Pts',(2.00000000049539,39.450000000286,-2.44929359890139E-16));
#6472=CARTESIAN_POINT('Ctrl Pts',(2.00000000049539,39.3916666669527,1.15470053866527));
#6473=CARTESIAN_POINT('Ctrl Pts',(1.0000000002477,39.3333333336194,1.7320508079979));
#6474=CARTESIAN_POINT('Ctrl Pts',(4.24230095595043E-16,39.275000000286,
2.30940107733053));
#6475=CARTESIAN_POINT('Ctrl Pts',(-1.0000000002477,39.2166666669527,1.7320508079979));
#6476=CARTESIAN_POINT('Ctrl Pts',(-2.00000000049539,39.1583333336194,1.15470053866527));
#6477=CARTESIAN_POINT('Ctrl Pts',(-2.00000000049539,39.100000000286,0.));
#6478=CARTESIAN_POINT('Ctrl Pts',(-2.00000000049539,39.0416666669527,-1.15470053866527));
#6479=CARTESIAN_POINT('Ctrl Pts',(-1.0000000002477,38.9833333336194,-1.7320508079979));
#6480=CARTESIAN_POINT('Ctrl Pts',(-1.41410031865014E-16,38.925000000286,
-2.30940107733053));
#6481=CARTESIAN_POINT('Ctrl Pts',(1.0000000002477,38.8666666669527,-1.7320508079979));
#6482=CARTESIAN_POINT('Ctrl Pts',(2.00000000049539,38.8083333336194,-1.15470053866527));
#6483=CARTESIAN_POINT('Ctrl Pts',(2.00000000049539,38.750000000286,-2.44929359890139E-16));
#6484=CARTESIAN_POINT('Ctrl Pts',(2.00000000049539,38.6916666669527,1.15470053866527));
#6485=CARTESIAN_POINT('Ctrl Pts',(1.0000000002477,38.6333333336194,1.7320508079979));
#6486=CARTESIAN_POINT('Ctrl Pts',(4.24230095595043E-16,38.575000000286,
2.30940107733053));
#6487=CARTESIAN_POINT('Ctrl Pts',(-1.0000000002477,38.5166666669527,1.7320508079979));
#6488=CARTESIAN_POINT('Ctrl Pts',(-2.00000000049539,38.4583333336194,1.15470053866527));
#6489=CARTESIAN_POINT('Ctrl Pts',(-2.00000000049539,38.400000000286,0.));
#6490=CARTESIAN_POINT('Ctrl Pts',(-2.00000000049539,38.3416666669527,-1.15470053866527));
#6491=CARTESIAN_POINT('Ctrl Pts',(-1.0000000002477,38.2833333336194,-1.7320508079979));
#6492=CARTESIAN_POINT('Ctrl Pts',(-1.41410031865014E-16,38.225000000286,
-2.30940107733053));
#6493=CARTESIAN_POINT('Ctrl Pts',(1.0000000002477,38.1666666669527,-1.7320508079979));
#6494=CARTESIAN_POINT('Ctrl Pts',(2.00000000049539,38.1083333336194,-1.15470053866527));
#6495=CARTESIAN_POINT('Ctrl Pts',(2.00000000049539,38.050000000286,-2.44929359890139E-16));
#6496=CARTESIAN_POINT('Ctrl Pts',(2.00000000049539,37.9916666669527,1.15470053866527));
#6497=CARTESIAN_POINT('Ctrl Pts',(1.0000000002477,37.9333333336194,1.7320508079979));
#6498=CARTESIAN_POINT('Ctrl Pts',(4.24230095595043E-16,37.875000000286,
2.30940107733053));
#6499=CARTESIAN_POINT('Ctrl Pts',(-1.0000000002477,37.8166666669527,1.7320508079979));
#6500=CARTESIAN_POINT('Ctrl Pts',(-2.00000000049539,37.7583333336194,1.15470053866527));
#6501=CARTESIAN_POINT('Ctrl Pts',(-2.00000000049539,37.700000000286,0.));
#6502=CARTESIAN_POINT('Ctrl Pts',(-2.00000000049539,37.6416666669527,-1.15470053866527));
#6503=CARTESIAN_POINT('Ctrl Pts',(-1.0000000002477,37.5833333336194,-1.7320508079979));
#6504=CARTESIAN_POINT('Ctrl Pts',(-1.41410031865014E-16,37.525000000286,
-2.30940107733053));
#6505=CARTESIAN_POINT('Ctrl Pts',(1.0000000002477,37.4666666669527,-1.7320508079979));
#6506=CARTESIAN_POINT('Ctrl Pts',(2.00000000049539,37.4083333336194,-1.15470053866527));
#6507=CARTESIAN_POINT('Ctrl Pts',(2.00000000049539,37.350000000286,-2.44929359890139E-16));
#6508=CARTESIAN_POINT('Ctrl Pts',(2.00000000049539,37.2916666669527,1.15470053866527));
#6509=CARTESIAN_POINT('Ctrl Pts',(1.0000000002477,37.2333333336194,1.7320508079979));
#6510=CARTESIAN_POINT('Ctrl Pts',(4.24230095595043E-16,37.175000000286,
2.30940107733053));
#6511=CARTESIAN_POINT('Ctrl Pts',(-1.0000000002477,37.1166666669527,1.7320508079979));
#6512=CARTESIAN_POINT('Ctrl Pts',(-2.00000000049539,37.0583333336194,1.15470053866527));
#6513=CARTESIAN_POINT('Ctrl Pts',(-2.00000000049539,37.000000000286,0.));
#6514=CARTESIAN_POINT('Ctrl Pts',(-2.00000000049539,36.9416666669527,-1.15470053866527));
#6515=CARTESIAN_POINT('Ctrl Pts',(-1.0000000002477,36.8833333336194,-1.7320508079979));
#6516=CARTESIAN_POINT('Ctrl Pts',(-1.41410031865014E-16,36.825000000286,
-2.30940107733053));
#6517=CARTESIAN_POINT('Ctrl Pts',(1.0000000002477,36.7666666669527,-1.7320508079979));
#6518=CARTESIAN_POINT('Ctrl Pts',(2.00000000049539,36.7083333336194,-1.15470053866527));
#6519=CARTESIAN_POINT('Ctrl Pts',(2.00000000049539,36.650000000286,-2.44929359890139E-16));
#6520=CARTESIAN_POINT('Ctrl Pts',(2.00000000049539,36.5916666669527,1.15470053866527));
#6521=CARTESIAN_POINT('Ctrl Pts',(1.0000000002477,36.5333333336194,1.7320508079979));
#6522=CARTESIAN_POINT('Ctrl Pts',(4.24230095595043E-16,36.475000000286,
2.30940107733053));
#6523=CARTESIAN_POINT('Ctrl Pts',(-1.0000000002477,36.4166666669527,1.7320508079979));
#6524=CARTESIAN_POINT('Ctrl Pts',(-2.00000000049539,36.3583333336194,1.15470053866527));
#6525=CARTESIAN_POINT('Ctrl Pts',(-2.00000000049539,36.300000000286,0.));
#6526=CARTESIAN_POINT('Ctrl Pts',(-2.00000000049539,36.2416666669527,-1.15470053866527));
#6527=CARTESIAN_POINT('Ctrl Pts',(-1.0000000002477,36.1833333336194,-1.7320508079979));
#6528=CARTESIAN_POINT('Ctrl Pts',(-1.41410031865014E-16,36.125000000286,
-2.30940107733053));
#6529=CARTESIAN_POINT('Ctrl Pts',(1.0000000002477,36.0666666669527,-1.7320508079979));
#6530=CARTESIAN_POINT('Ctrl Pts',(2.00000000049539,36.0083333336194,-1.15470053866527));
#6531=CARTESIAN_POINT('Ctrl Pts',(2.00000000049539,35.950000000286,-2.44929359890139E-16));
#6532=CARTESIAN_POINT('Ctrl Pts',(2.00000000049539,35.8916666669527,1.15470053866527));
#6533=CARTESIAN_POINT('Ctrl Pts',(1.0000000002477,35.8333333336194,1.7320508079979));
#6534=CARTESIAN_POINT('Ctrl Pts',(4.24230095595043E-16,35.775000000286,
2.30940107733053));
#6535=CARTESIAN_POINT('Ctrl Pts',(-1.0000000002477,35.7166666669527,1.7320508079979));
#6536=CARTESIAN_POINT('Ctrl Pts',(-2.00000000049539,35.6583333336194,1.15470053866527));
#6537=CARTESIAN_POINT('Ctrl Pts',(-2.00000000049539,35.600000000286,0.));
#6538=CARTESIAN_POINT('Ctrl Pts',(-2.00000000049539,35.5416666669527,-1.15470053866527));
#6539=CARTESIAN_POINT('Ctrl Pts',(-1.0000000002477,35.4833333336194,-1.7320508079979));
#6540=CARTESIAN_POINT('Ctrl Pts',(-1.41410031865014E-16,35.425000000286,
-2.30940107733053));
#6541=CARTESIAN_POINT('Ctrl Pts',(1.0000000002477,35.3666666669527,-1.7320508079979));
#6542=CARTESIAN_POINT('Ctrl Pts',(2.00000000049539,35.3083333336194,-1.15470053866527));
#6543=CARTESIAN_POINT('Ctrl Pts',(2.00000000049539,35.250000000286,-2.44929359890139E-16));
#6544=CARTESIAN_POINT('Ctrl Pts',(2.00000000049539,35.1916666669527,1.15470053866527));
#6545=CARTESIAN_POINT('Ctrl Pts',(1.0000000002477,35.1333333336194,1.7320508079979));
#6546=CARTESIAN_POINT('Ctrl Pts',(4.24230095595043E-16,35.075000000286,
2.30940107733053));
#6547=CARTESIAN_POINT('Ctrl Pts',(-1.0000000002477,35.0166666669527,1.7320508079979));
#6548=CARTESIAN_POINT('Ctrl Pts',(-2.00000000049539,34.9583333336194,1.15470053866527));
#6549=CARTESIAN_POINT('Ctrl Pts',(-2.00000000049539,34.900000000286,0.));
#6550=CARTESIAN_POINT('Ctrl Pts',(-2.00000000049539,34.8416666669527,-1.15470053866527));
#6551=CARTESIAN_POINT('Ctrl Pts',(-1.0000000002477,34.7833333336194,-1.7320508079979));
#6552=CARTESIAN_POINT('Ctrl Pts',(-1.41410031865014E-16,34.725000000286,
-2.30940107733053));
#6553=CARTESIAN_POINT('Ctrl Pts',(1.0000000002477,34.6666666669527,-1.7320508079979));
#6554=CARTESIAN_POINT('Ctrl Pts',(2.00000000049539,34.6083333336194,-1.15470053866527));
#6555=CARTESIAN_POINT('Ctrl Pts',(2.00000000049539,34.550000000286,-2.44929359890139E-16));
#6556=CARTESIAN_POINT('Ctrl Pts',(2.00000000049539,34.4916666669527,1.15470053866527));
#6557=CARTESIAN_POINT('Ctrl Pts',(1.0000000002477,34.4333333336194,1.7320508079979));
#6558=CARTESIAN_POINT('Ctrl Pts',(4.24230095595043E-16,34.375000000286,
2.30940107733053));
#6559=CARTESIAN_POINT('Ctrl Pts',(-1.0000000002477,34.3166666669527,1.7320508079979));
#6560=CARTESIAN_POINT('Ctrl Pts',(-2.00000000049539,34.2583333336194,1.15470053866527));
#6561=CARTESIAN_POINT('Ctrl Pts',(-2.00000000049539,34.200000000286,0.));
#6562=CARTESIAN_POINT('Ctrl Pts',(-2.00000000049539,34.1416666669527,-1.15470053866527));
#6563=CARTESIAN_POINT('Ctrl Pts',(-1.0000000002477,34.0833333336194,-1.7320508079979));
#6564=CARTESIAN_POINT('Ctrl Pts',(-1.41410031865014E-16,34.025000000286,
-2.30940107733053));
#6565=CARTESIAN_POINT('Ctrl Pts',(1.0000000002477,33.9666666669527,-1.7320508079979));
#6566=CARTESIAN_POINT('Ctrl Pts',(2.00000000049539,33.9083333336194,-1.15470053866527));
#6567=CARTESIAN_POINT('Ctrl Pts',(2.00000000049539,33.850000000286,-2.44929359890139E-16));
#6568=CARTESIAN_POINT('Ctrl Pts',(2.00000000049539,33.7916666669527,1.15470053866527));
#6569=CARTESIAN_POINT('Ctrl Pts',(1.0000000002477,33.7333333336194,1.7320508079979));
#6570=CARTESIAN_POINT('Ctrl Pts',(4.24230095595043E-16,33.675000000286,
2.30940107733053));
#6571=CARTESIAN_POINT('Ctrl Pts',(-1.0000000002477,33.6166666669527,1.7320508079979));
#6572=CARTESIAN_POINT('Ctrl Pts',(-2.00000000049539,33.5583333336194,1.15470053866527));
#6573=CARTESIAN_POINT('Ctrl Pts',(-2.00000000049539,33.500000000286,0.));
#6574=CARTESIAN_POINT('Ctrl Pts',(-2.00000000049539,33.4416666669527,-1.15470053866527));
#6575=CARTESIAN_POINT('Ctrl Pts',(-1.0000000002477,33.3833333336194,-1.7320508079979));
#6576=CARTESIAN_POINT('Ctrl Pts',(-1.41410031865014E-16,33.325000000286,
-2.30940107733053));
#6577=CARTESIAN_POINT('Ctrl Pts',(1.0000000002477,33.2666666669527,-1.7320508079979));
#6578=CARTESIAN_POINT('Ctrl Pts',(2.00000000049539,33.2083333336194,-1.15470053866527));
#6579=CARTESIAN_POINT('Ctrl Pts',(2.00000000049539,33.150000000286,-2.44929359890139E-16));
#6580=CARTESIAN_POINT('Ctrl Pts',(2.00000000049539,33.0916666669527,1.15470053866527));
#6581=CARTESIAN_POINT('Ctrl Pts',(1.0000000002477,33.0333333336194,1.7320508079979));
#6582=CARTESIAN_POINT('Ctrl Pts',(4.24230095595043E-16,32.975000000286,
2.30940107733053));
#6583=CARTESIAN_POINT('Ctrl Pts',(-1.0000000002477,32.9166666669527,1.7320508079979));
#6584=CARTESIAN_POINT('Ctrl Pts',(-2.00000000049539,32.8583333336194,1.15470053866527));
#6585=CARTESIAN_POINT('Ctrl Pts',(-2.00000000049539,32.800000000286,0.));
#6586=CARTESIAN_POINT('Ctrl Pts',(-2.00000000049539,32.7416666669527,-1.15470053866527));
#6587=CARTESIAN_POINT('Ctrl Pts',(-1.0000000002477,32.6833333336194,-1.7320508079979));
#6588=CARTESIAN_POINT('Ctrl Pts',(-1.41410031865014E-16,32.625000000286,
-2.30940107733053));
#6589=CARTESIAN_POINT('Ctrl Pts',(1.0000000002477,32.5666666669527,-1.7320508079979));
#6590=CARTESIAN_POINT('Ctrl Pts',(2.00000000049539,32.5083333336194,-1.15470053866527));
#6591=CARTESIAN_POINT('Ctrl Pts',(2.00000000049539,32.450000000286,-2.44929359890139E-16));
#6592=CARTESIAN_POINT('Ctrl Pts',(2.00000000049539,32.3916666669527,1.15470053866527));
#6593=CARTESIAN_POINT('Ctrl Pts',(1.0000000002477,32.3333333336194,1.7320508079979));
#6594=CARTESIAN_POINT('Ctrl Pts',(4.24230095595043E-16,32.275000000286,
2.30940107733053));
#6595=CARTESIAN_POINT('Ctrl Pts',(-1.0000000002477,32.2166666669527,1.7320508079979));
#6596=CARTESIAN_POINT('Ctrl Pts',(-2.00000000049539,32.1583333336194,1.15470053866527));
#6597=CARTESIAN_POINT('Ctrl Pts',(-2.00000000049539,32.100000000286,0.));
#6598=CARTESIAN_POINT('Ctrl Pts',(-2.00000000049539,32.0416666669527,-1.15470053866527));
#6599=CARTESIAN_POINT('Ctrl Pts',(-1.0000000002477,31.9833333336194,-1.7320508079979));
#6600=CARTESIAN_POINT('Ctrl Pts',(-1.41410031865014E-16,31.925000000286,
-2.30940107733053));
#6601=CARTESIAN_POINT('Ctrl Pts',(1.0000000002477,31.8666666669527,-1.7320508079979));
#6602=CARTESIAN_POINT('Ctrl Pts',(2.00000000049539,31.8083333336194,-1.15470053866527));
#6603=CARTESIAN_POINT('Ctrl Pts',(2.00000000049539,31.750000000286,-2.44929359890139E-16));
#6604=CARTESIAN_POINT('Ctrl Pts',(2.00000000049539,31.6916666669527,1.15470053866527));
#6605=CARTESIAN_POINT('Ctrl Pts',(1.0000000002477,31.6333333336194,1.7320508079979));
#6606=CARTESIAN_POINT('Ctrl Pts',(4.24230095595043E-16,31.575000000286,
2.30940107733053));
#6607=CARTESIAN_POINT('Ctrl Pts',(-1.0000000002477,31.5166666669527,1.7320508079979));
#6608=CARTESIAN_POINT('Ctrl Pts',(-2.00000000049539,31.4583333336194,1.15470053866527));
#6609=CARTESIAN_POINT('Ctrl Pts',(-2.00000000049539,31.400000000286,0.));
#6610=CARTESIAN_POINT('Ctrl Pts',(-2.00000000049539,31.3416666669527,-1.15470053866527));
#6611=CARTESIAN_POINT('Ctrl Pts',(-1.0000000002477,31.2833333336194,-1.7320508079979));
#6612=CARTESIAN_POINT('Ctrl Pts',(-1.41410031865014E-16,31.225000000286,
-2.30940107733053));
#6613=CARTESIAN_POINT('Ctrl Pts',(1.0000000002477,31.1666666669527,-1.7320508079979));
#6614=CARTESIAN_POINT('Ctrl Pts',(2.00000000049539,31.1083333336194,-1.15470053866527));
#6615=CARTESIAN_POINT('Ctrl Pts',(2.00000000049539,31.050000000286,-2.44929359890139E-16));
#6616=CARTESIAN_POINT('Ctrl Pts',(2.00000000049539,30.9916666669527,1.15470053866527));
#6617=CARTESIAN_POINT('Ctrl Pts',(1.0000000002477,30.9333333336194,1.7320508079979));
#6618=CARTESIAN_POINT('Ctrl Pts',(4.24230095595043E-16,30.875000000286,
2.30940107733053));
#6619=CARTESIAN_POINT('Ctrl Pts',(-1.0000000002477,30.8166666669527,1.7320508079979));
#6620=CARTESIAN_POINT('Ctrl Pts',(-2.00000000049539,30.7583333336194,1.15470053866527));
#6621=CARTESIAN_POINT('Ctrl Pts',(-2.00000000049539,30.700000000286,0.));
#6622=CARTESIAN_POINT('Ctrl Pts',(-2.00000000049539,30.6416666669527,-1.15470053866527));
#6623=CARTESIAN_POINT('Ctrl Pts',(-1.0000000002477,30.5833333336194,-1.7320508079979));
#6624=CARTESIAN_POINT('Ctrl Pts',(-1.41410031865014E-16,30.525000000286,
-2.30940107733053));
#6625=CARTESIAN_POINT('Ctrl Pts',(1.0000000002477,30.4666666669527,-1.7320508079979));
#6626=CARTESIAN_POINT('Ctrl Pts',(2.00000000049539,30.4083333336193,-1.15470053866527));
#6627=CARTESIAN_POINT('Ctrl Pts',(2.00000000049539,30.350000000286,-2.44929359890139E-16));
#6628=CARTESIAN_POINT('Ctrl Pts',(2.00000000049539,30.2916666669527,1.15470053866527));
#6629=CARTESIAN_POINT('Ctrl Pts',(1.0000000002477,30.2333333336194,1.7320508079979));
#6630=CARTESIAN_POINT('Ctrl Pts',(4.24230095595043E-16,30.175000000286,
2.30940107733053));
#6631=CARTESIAN_POINT('Ctrl Pts',(-1.0000000002477,30.1166666669527,1.7320508079979));
#6632=CARTESIAN_POINT('Ctrl Pts',(-2.00000000049539,30.0583333336194,1.15470053866527));
#6633=CARTESIAN_POINT('Ctrl Pts',(-2.00000000049539,30.000000000286,0.));
#6634=CARTESIAN_POINT('Ctrl Pts',(-2.00000000049539,29.9416666669527,-1.15470053866527));
#6635=CARTESIAN_POINT('Ctrl Pts',(-1.0000000002477,29.8833333336194,-1.7320508079979));
#6636=CARTESIAN_POINT('Ctrl Pts',(-1.41410031865014E-16,29.825000000286,
-2.30940107733053));
#6637=CARTESIAN_POINT('Ctrl Pts',(1.0000000002477,29.7666666669527,-1.7320508079979));
#6638=CARTESIAN_POINT('Ctrl Pts',(2.00000000049539,29.7083333336194,-1.15470053866527));
#6639=CARTESIAN_POINT('Ctrl Pts',(2.00000000049539,29.650000000286,-2.44929359890139E-16));
#6640=CARTESIAN_POINT('Ctrl Pts',(2.00000000049539,29.5916666669527,1.15470053866527));
#6641=CARTESIAN_POINT('Ctrl Pts',(1.0000000002477,29.5333333336194,1.7320508079979));
#6642=CARTESIAN_POINT('Ctrl Pts',(4.24230095595043E-16,29.475000000286,
2.30940107733053));
#6643=CARTESIAN_POINT('Ctrl Pts',(-1.0000000002477,29.4166666669527,1.7320508079979));
#6644=CARTESIAN_POINT('Ctrl Pts',(-2.00000000049539,29.3583333336194,1.15470053866527));
#6645=CARTESIAN_POINT('Ctrl Pts',(-2.00000000049539,29.300000000286,0.));
#6646=CARTESIAN_POINT('Ctrl Pts',(-2.00000000049539,29.2416666669527,-1.15470053866527));
#6647=CARTESIAN_POINT('Ctrl Pts',(-1.0000000002477,29.1833333336194,-1.7320508079979));
#6648=CARTESIAN_POINT('Ctrl Pts',(-1.41410031865014E-16,29.125000000286,
-2.30940107733053));
#6649=CARTESIAN_POINT('Ctrl Pts',(1.0000000002477,29.0666666669527,-1.7320508079979));
#6650=CARTESIAN_POINT('Ctrl Pts',(2.00000000049539,29.0083333336194,-1.15470053866527));
#6651=CARTESIAN_POINT('Ctrl Pts',(2.00000000049539,28.950000000286,-2.44929359890139E-16));
#6652=CARTESIAN_POINT('Ctrl Pts',(2.00000000049539,28.8916666669527,1.15470053866527));
#6653=CARTESIAN_POINT('Ctrl Pts',(1.0000000002477,28.8333333336194,1.7320508079979));
#6654=CARTESIAN_POINT('Ctrl Pts',(4.24230095595043E-16,28.775000000286,
2.30940107733053));
#6655=CARTESIAN_POINT('Ctrl Pts',(-1.0000000002477,28.7166666669527,1.7320508079979));
#6656=CARTESIAN_POINT('Ctrl Pts',(-2.00000000049539,28.6583333336194,1.15470053866527));
#6657=CARTESIAN_POINT('Ctrl Pts',(-2.00000000049539,28.600000000286,0.));
#6658=CARTESIAN_POINT('Ctrl Pts',(-2.00000000049539,28.5416666669527,-1.15470053866527));
#6659=CARTESIAN_POINT('Ctrl Pts',(-1.0000000002477,28.4833333336194,-1.7320508079979));
#6660=CARTESIAN_POINT('Ctrl Pts',(-1.41410031865014E-16,28.425000000286,
-2.30940107733053));
#6661=CARTESIAN_POINT('Ctrl Pts',(1.0000000002477,28.3666666669527,-1.7320508079979));
#6662=CARTESIAN_POINT('Ctrl Pts',(2.00000000049539,28.3083333336194,-1.15470053866527));
#6663=CARTESIAN_POINT('Ctrl Pts',(2.00000000049539,28.250000000286,-2.44929359890139E-16));
#6664=CARTESIAN_POINT('Ctrl Pts',(2.00000000049539,28.1916666669527,1.15470053866527));
#6665=CARTESIAN_POINT('Ctrl Pts',(1.0000000002477,28.1333333336194,1.7320508079979));
#6666=CARTESIAN_POINT('Ctrl Pts',(4.24230095595043E-16,28.075000000286,
2.30940107733053));
#6667=CARTESIAN_POINT('Ctrl Pts',(-1.0000000002477,28.0166666669527,1.7320508079979));
#6668=CARTESIAN_POINT('Ctrl Pts',(-2.00000000049539,27.9583333336194,1.15470053866527));
#6669=CARTESIAN_POINT('Ctrl Pts',(-2.00000000049539,27.900000000286,0.));
#6670=CARTESIAN_POINT('Ctrl Pts',(-2.00000000049539,27.8416666669527,-1.15470053866527));
#6671=CARTESIAN_POINT('Ctrl Pts',(-1.0000000002477,27.7833333336194,-1.7320508079979));
#6672=CARTESIAN_POINT('Ctrl Pts',(-1.41410031865014E-16,27.725000000286,
-2.30940107733053));
#6673=CARTESIAN_POINT('Ctrl Pts',(1.0000000002477,27.6666666669527,-1.7320508079979));
#6674=CARTESIAN_POINT('Ctrl Pts',(2.00000000049539,27.6083333336194,-1.15470053866527));
#6675=CARTESIAN_POINT('Ctrl Pts',(2.00000000049539,27.550000000286,-2.44929359890139E-16));
#6676=CARTESIAN_POINT('Ctrl Pts',(2.00000000049539,27.4916666669527,1.15470053866527));
#6677=CARTESIAN_POINT('Ctrl Pts',(1.0000000002477,27.4333333336194,1.7320508079979));
#6678=CARTESIAN_POINT('Ctrl Pts',(4.24230095595043E-16,27.375000000286,
2.30940107733053));
#6679=CARTESIAN_POINT('Ctrl Pts',(-1.0000000002477,27.3166666669527,1.7320508079979));
#6680=CARTESIAN_POINT('Ctrl Pts',(-2.00000000049539,27.2583333336194,1.15470053866527));
#6681=CARTESIAN_POINT('Ctrl Pts',(-2.00000000049539,27.200000000286,0.));
#6682=CARTESIAN_POINT('Ctrl Pts',(-2.00000000049539,27.1416666669527,-1.15470053866527));
#6683=CARTESIAN_POINT('Ctrl Pts',(-1.0000000002477,27.0833333336194,-1.7320508079979));
#6684=CARTESIAN_POINT('Ctrl Pts',(-1.41410031865014E-16,27.025000000286,
-2.30940107733053));
#6685=CARTESIAN_POINT('Ctrl Pts',(1.0000000002477,26.9666666669527,-1.7320508079979));
#6686=CARTESIAN_POINT('Ctrl Pts',(2.00000000049539,26.9083333336194,-1.15470053866527));
#6687=CARTESIAN_POINT('Ctrl Pts',(2.00000000049539,26.850000000286,-2.44929359890139E-16));
#6688=CARTESIAN_POINT('Ctrl Pts',(2.00000000049539,26.7916666669527,1.15470053866527));
#6689=CARTESIAN_POINT('Ctrl Pts',(1.0000000002477,26.7333333336194,1.7320508079979));
#6690=CARTESIAN_POINT('Ctrl Pts',(4.24230095595043E-16,26.675000000286,
2.30940107733053));
#6691=CARTESIAN_POINT('Ctrl Pts',(-1.0000000002477,26.6166666669527,1.7320508079979));
#6692=CARTESIAN_POINT('Ctrl Pts',(-2.00000000049539,26.5583333336194,1.15470053866527));
#6693=CARTESIAN_POINT('Ctrl Pts',(-2.00000000049539,26.500000000286,0.));
#6694=CARTESIAN_POINT('Ctrl Pts',(-2.00000000049539,26.4416666669527,-1.15470053866527));
#6695=CARTESIAN_POINT('Ctrl Pts',(-1.0000000002477,26.3833333336194,-1.7320508079979));
#6696=CARTESIAN_POINT('Ctrl Pts',(-1.41410031865014E-16,26.325000000286,
-2.30940107733053));
#6697=CARTESIAN_POINT('Ctrl Pts',(1.0000000002477,26.2666666669527,-1.7320508079979));
#6698=CARTESIAN_POINT('Ctrl Pts',(2.00000000049539,26.2083333336194,-1.15470053866527));
#6699=CARTESIAN_POINT('Ctrl Pts',(2.00000000049539,26.150000000286,-2.44929359890139E-16));
#6700=CARTESIAN_POINT('Ctrl Pts',(2.00000000049539,26.0916666669527,1.15470053866527));
#6701=CARTESIAN_POINT('Ctrl Pts',(1.0000000002477,26.0333333336194,1.7320508079979));
#6702=CARTESIAN_POINT('Ctrl Pts',(4.24230095595043E-16,25.975000000286,
2.30940107733053));
#6703=CARTESIAN_POINT('Ctrl Pts',(-1.0000000002477,25.9166666669527,1.7320508079979));
#6704=CARTESIAN_POINT('Ctrl Pts',(-2.00000000049539,25.8583333336194,1.15470053866527));
#6705=CARTESIAN_POINT('Ctrl Pts',(-2.00000000049539,25.800000000286,0.));
#6706=CARTESIAN_POINT('Ctrl Pts',(-2.00000000049539,25.7416666669527,-1.15470053866527));
#6707=CARTESIAN_POINT('Ctrl Pts',(-1.0000000002477,25.6833333336194,-1.7320508079979));
#6708=CARTESIAN_POINT('Ctrl Pts',(-1.41410031865014E-16,25.625000000286,
-2.30940107733053));
#6709=CARTESIAN_POINT('Ctrl Pts',(1.0000000002477,25.5666666669527,-1.7320508079979));
#6710=CARTESIAN_POINT('Ctrl Pts',(2.00000000049539,25.5083333336194,-1.15470053866527));
#6711=CARTESIAN_POINT('Ctrl Pts',(2.00000000049539,25.450000000286,-2.44929359890139E-16));
#6712=CARTESIAN_POINT('Ctrl Pts',(2.00000000049539,25.3916666669527,1.15470053866527));
#6713=CARTESIAN_POINT('Ctrl Pts',(1.0000000002477,25.3333333336194,1.7320508079979));
#6714=CARTESIAN_POINT('Ctrl Pts',(4.24230095595043E-16,25.275000000286,
2.30940107733053));
#6715=CARTESIAN_POINT('Ctrl Pts',(-1.0000000002477,25.2166666669527,1.7320508079979));
#6716=CARTESIAN_POINT('Ctrl Pts',(-2.00000000049539,25.1583333336194,1.15470053866527));
#6717=CARTESIAN_POINT('Ctrl Pts',(-2.00000000049539,25.100000000286,0.));
#6718=CARTESIAN_POINT('Ctrl Pts',(-2.00000000049539,25.0416666669527,-1.15470053866527));
#6719=CARTESIAN_POINT('Ctrl Pts',(-1.0000000002477,24.9833333336194,-1.7320508079979));
#6720=CARTESIAN_POINT('Ctrl Pts',(-1.41410031865014E-16,24.925000000286,
-2.30940107733053));
#6721=CARTESIAN_POINT('Ctrl Pts',(1.0000000002477,24.8666666669527,-1.7320508079979));
#6722=CARTESIAN_POINT('Ctrl Pts',(2.00000000049539,24.8083333336194,-1.15470053866527));
#6723=CARTESIAN_POINT('Ctrl Pts',(2.00000000049539,24.750000000286,-2.44929359890139E-16));
#6724=CARTESIAN_POINT('Ctrl Pts',(2.00000000049539,24.6916666669527,1.15470053866527));
#6725=CARTESIAN_POINT('Ctrl Pts',(1.0000000002477,24.6333333336194,1.7320508079979));
#6726=CARTESIAN_POINT('Ctrl Pts',(4.24230095595043E-16,24.575000000286,
2.30940107733053));
#6727=CARTESIAN_POINT('Ctrl Pts',(-1.0000000002477,24.5166666669527,1.7320508079979));
#6728=CARTESIAN_POINT('Ctrl Pts',(-2.00000000049539,24.4583333336194,1.15470053866527));
#6729=CARTESIAN_POINT('Ctrl Pts',(-2.00000000049539,24.400000000286,0.));
#6730=CARTESIAN_POINT('Ctrl Pts',(-2.00000000049539,24.3416666669527,-1.15470053866527));
#6731=CARTESIAN_POINT('Ctrl Pts',(-1.0000000002477,24.2833333336194,-1.7320508079979));
#6732=CARTESIAN_POINT('Ctrl Pts',(-1.41410031865014E-16,24.225000000286,
-2.30940107733053));
#6733=CARTESIAN_POINT('Ctrl Pts',(1.0000000002477,24.1666666669527,-1.7320508079979));
#6734=CARTESIAN_POINT('Ctrl Pts',(2.00000000049539,24.1083333336194,-1.15470053866527));
#6735=CARTESIAN_POINT('Ctrl Pts',(2.00000000049539,24.050000000286,-2.44929359890139E-16));
#6736=CARTESIAN_POINT('Ctrl Pts',(2.00000000049539,23.9916666669527,1.15470053866527));
#6737=CARTESIAN_POINT('Ctrl Pts',(1.0000000002477,23.9333333336194,1.7320508079979));
#6738=CARTESIAN_POINT('Ctrl Pts',(4.24230095595043E-16,23.875000000286,
2.30940107733053));
#6739=CARTESIAN_POINT('Ctrl Pts',(-1.0000000002477,23.8166666669527,1.7320508079979));
#6740=CARTESIAN_POINT('Ctrl Pts',(-2.00000000049539,23.7583333336194,1.15470053866527));
#6741=CARTESIAN_POINT('Ctrl Pts',(-2.00000000049539,23.700000000286,0.));
#6742=CARTESIAN_POINT('Ctrl Pts',(-2.00000000049539,23.6416666669527,-1.15470053866527));
#6743=CARTESIAN_POINT('Ctrl Pts',(-1.0000000002477,23.5833333336194,-1.7320508079979));
#6744=CARTESIAN_POINT('Ctrl Pts',(-1.41410031865014E-16,23.525000000286,
-2.30940107733053));
#6745=CARTESIAN_POINT('Ctrl Pts',(1.0000000002477,23.4666666669527,-1.7320508079979));
#6746=CARTESIAN_POINT('Ctrl Pts',(2.00000000049539,23.4083333336194,-1.15470053866527));
#6747=CARTESIAN_POINT('Ctrl Pts',(2.00000000049539,23.350000000286,-2.44929359890139E-16));
#6748=CARTESIAN_POINT('Ctrl Pts',(2.00000000049539,23.2916666669527,1.15470053866527));
#6749=CARTESIAN_POINT('Ctrl Pts',(1.0000000002477,23.2333333336194,1.7320508079979));
#6750=CARTESIAN_POINT('Ctrl Pts',(4.24230095595043E-16,23.175000000286,
2.30940107733053));
#6751=CARTESIAN_POINT('Ctrl Pts',(-1.0000000002477,23.1166666669527,1.7320508079979));
#6752=CARTESIAN_POINT('Ctrl Pts',(-2.00000000049539,23.0583333336194,1.15470053866527));
#6753=CARTESIAN_POINT('Ctrl Pts',(-2.00000000049539,23.000000000286,0.));
#6754=CARTESIAN_POINT('Ctrl Pts',(-2.00000000049539,22.9416666669527,-1.15470053866527));
#6755=CARTESIAN_POINT('Ctrl Pts',(-1.0000000002477,22.8833333336194,-1.7320508079979));
#6756=CARTESIAN_POINT('Ctrl Pts',(-1.41410031865014E-16,22.825000000286,
-2.30940107733053));
#6757=CARTESIAN_POINT('Ctrl Pts',(1.0000000002477,22.7666666669527,-1.7320508079979));
#6758=CARTESIAN_POINT('Ctrl Pts',(2.00000000049539,22.7083333336194,-1.15470053866527));
#6759=CARTESIAN_POINT('Ctrl Pts',(2.00000000049539,22.650000000286,-2.44929359890139E-16));
#6760=CARTESIAN_POINT('Ctrl Pts',(2.00000000049539,22.5916666669527,1.15470053866527));
#6761=CARTESIAN_POINT('Ctrl Pts',(1.0000000002477,22.5333333336194,1.7320508079979));
#6762=CARTESIAN_POINT('Ctrl Pts',(4.24230095595043E-16,22.475000000286,
2.30940107733053));
#6763=CARTESIAN_POINT('Ctrl Pts',(-1.0000000002477,22.4166666669527,1.7320508079979));
#6764=CARTESIAN_POINT('Ctrl Pts',(-2.00000000049539,22.3583333336194,1.15470053866527));
#6765=CARTESIAN_POINT('Ctrl Pts',(-2.00000000049539,22.300000000286,0.));
#6766=CARTESIAN_POINT('Ctrl Pts',(-2.00000000049539,22.2416666669527,-1.15470053866527));
#6767=CARTESIAN_POINT('Ctrl Pts',(-1.0000000002477,22.1833333336194,-1.7320508079979));
#6768=CARTESIAN_POINT('Ctrl Pts',(-1.41410031865014E-16,22.125000000286,
-2.30940107733053));
#6769=CARTESIAN_POINT('Ctrl Pts',(1.0000000002477,22.0666666669527,-1.7320508079979));
#6770=CARTESIAN_POINT('Ctrl Pts',(2.00000000049539,22.0083333336194,-1.15470053866527));
#6771=CARTESIAN_POINT('Ctrl Pts',(2.00000000049539,21.950000000286,-2.44929359890139E-16));
#6772=CARTESIAN_POINT('Ctrl Pts',(2.00000000049539,21.8916666669527,1.15470053866527));
#6773=CARTESIAN_POINT('Ctrl Pts',(1.0000000002477,21.8333333336194,1.7320508079979));
#6774=CARTESIAN_POINT('Ctrl Pts',(4.24230095595043E-16,21.775000000286,
2.30940107733053));
#6775=CARTESIAN_POINT('Ctrl Pts',(-1.0000000002477,21.7166666669527,1.7320508079979));
#6776=CARTESIAN_POINT('Ctrl Pts',(-2.00000000049539,21.6583333336193,1.15470053866527));
#6777=CARTESIAN_POINT('Ctrl Pts',(-2.00000000049539,21.600000000286,0.));
#6778=CARTESIAN_POINT('Ctrl Pts',(-2.00000000049539,21.5416666669527,-1.15470053866527));
#6779=CARTESIAN_POINT('Ctrl Pts',(-1.0000000002477,21.4833333336194,-1.7320508079979));
#6780=CARTESIAN_POINT('Ctrl Pts',(-1.41410031865014E-16,21.425000000286,
-2.30940107733053));
#6781=CARTESIAN_POINT('Ctrl Pts',(1.0000000002477,21.3666666669527,-1.7320508079979));
#6782=CARTESIAN_POINT('Ctrl Pts',(2.00000000049539,21.3083333336193,-1.15470053866527));
#6783=CARTESIAN_POINT('Ctrl Pts',(2.00000000049539,21.250000000286,-2.44929359890139E-16));
#6784=CARTESIAN_POINT('Ctrl Pts',(2.00000000049539,21.1916666669527,1.15470053866527));
#6785=CARTESIAN_POINT('Ctrl Pts',(1.0000000002477,21.1333333336194,1.7320508079979));
#6786=CARTESIAN_POINT('Ctrl Pts',(4.24230095595043E-16,21.075000000286,
2.30940107733053));
#6787=CARTESIAN_POINT('Ctrl Pts',(-1.0000000002477,21.0166666669527,1.7320508079979));
#6788=CARTESIAN_POINT('Ctrl Pts',(-2.00000000049539,20.9583333336194,1.15470053866527));
#6789=CARTESIAN_POINT('Ctrl Pts',(-2.00000000049539,20.900000000286,0.));
#6790=CARTESIAN_POINT('Ctrl Pts',(-2.00000000049539,20.8416666669527,-1.15470053866527));
#6791=CARTESIAN_POINT('Ctrl Pts',(-1.0000000002477,20.7833333336194,-1.7320508079979));
#6792=CARTESIAN_POINT('Ctrl Pts',(-1.41410031865014E-16,20.725000000286,
-2.30940107733053));
#6793=CARTESIAN_POINT('Ctrl Pts',(1.0000000002477,20.6666666669527,-1.7320508079979));
#6794=CARTESIAN_POINT('Ctrl Pts',(2.00000000049539,20.6083333336194,-1.15470053866527));
#6795=CARTESIAN_POINT('Ctrl Pts',(2.00000000049539,20.550000000286,-2.44929359890139E-16));
#6796=CARTESIAN_POINT('Ctrl Pts',(2.00000000049539,20.4916666669527,1.15470053866527));
#6797=CARTESIAN_POINT('Ctrl Pts',(1.0000000002477,20.4333333336194,1.7320508079979));
#6798=CARTESIAN_POINT('Ctrl Pts',(4.24230095595043E-16,20.375000000286,
2.30940107733053));
#6799=CARTESIAN_POINT('Ctrl Pts',(-1.0000000002477,20.3166666669527,1.7320508079979));
#6800=CARTESIAN_POINT('Ctrl Pts',(-2.00000000049539,20.2583333336194,1.15470053866527));
#6801=CARTESIAN_POINT('Ctrl Pts',(-2.00000000049539,20.200000000286,0.));
#6802=CARTESIAN_POINT('Ctrl Pts',(-2.00000000049539,20.1416666669527,-1.15470053866527));
#6803=CARTESIAN_POINT('Ctrl Pts',(-1.0000000002477,20.0833333336194,-1.7320508079979));
#6804=CARTESIAN_POINT('Ctrl Pts',(-1.41410031865014E-16,20.025000000286,
-2.30940107733053));
#6805=CARTESIAN_POINT('Ctrl Pts',(1.0000000002477,19.9666666669527,-1.7320508079979));
#6806=CARTESIAN_POINT('Ctrl Pts',(2.00000000049539,19.9083333336194,-1.15470053866527));
#6807=CARTESIAN_POINT('Ctrl Pts',(2.00000000049539,19.850000000286,-2.44929359890139E-16));
#6808=CARTESIAN_POINT('Ctrl Pts',(2.00000000049539,19.7916666669527,1.15470053866527));
#6809=CARTESIAN_POINT('Ctrl Pts',(1.0000000002477,19.7333333336194,1.7320508079979));
#6810=CARTESIAN_POINT('Ctrl Pts',(4.24230095595043E-16,19.675000000286,
2.30940107733053));
#6811=CARTESIAN_POINT('Ctrl Pts',(-1.0000000002477,19.6166666669527,1.7320508079979));
#6812=CARTESIAN_POINT('Ctrl Pts',(-2.00000000049539,19.5583333336194,1.15470053866527));
#6813=CARTESIAN_POINT('Ctrl Pts',(-2.00000000049539,19.500000000286,0.));
#6814=CARTESIAN_POINT('Ctrl Pts',(-2.00000000049539,19.4416666669527,-1.15470053866527));
#6815=CARTESIAN_POINT('Ctrl Pts',(-1.0000000002477,19.3833333336194,-1.7320508079979));
#6816=CARTESIAN_POINT('Ctrl Pts',(-1.41410031865014E-16,19.325000000286,
-2.30940107733053));
#6817=CARTESIAN_POINT('Ctrl Pts',(1.0000000002477,19.2666666669527,-1.7320508079979));
#6818=CARTESIAN_POINT('Ctrl Pts',(2.00000000049539,19.2083333336194,-1.15470053866527));
#6819=CARTESIAN_POINT('Ctrl Pts',(2.00000000049539,19.150000000286,-2.44929359890139E-16));
#6820=CARTESIAN_POINT('Ctrl Pts',(2.00000000049539,19.0916666669527,1.15470053866527));
#6821=CARTESIAN_POINT('Ctrl Pts',(1.0000000002477,19.0333333336194,1.7320508079979));
#6822=CARTESIAN_POINT('Ctrl Pts',(4.24230095595043E-16,18.975000000286,
2.30940107733053));
#6823=CARTESIAN_POINT('Ctrl Pts',(-1.0000000002477,18.9166666669527,1.7320508079979));
#6824=CARTESIAN_POINT('Ctrl Pts',(-2.00000000049539,18.8583333336194,1.15470053866527));
#6825=CARTESIAN_POINT('Ctrl Pts',(-2.00000000049539,18.800000000286,0.));
#6826=CARTESIAN_POINT('Ctrl Pts',(-2.00000000049539,18.7416666669527,-1.15470053866527));
#6827=CARTESIAN_POINT('Ctrl Pts',(-1.0000000002477,18.6833333336194,-1.7320508079979));
#6828=CARTESIAN_POINT('Ctrl Pts',(-1.41410031865014E-16,18.625000000286,
-2.30940107733053));
#6829=CARTESIAN_POINT('Ctrl Pts',(1.0000000002477,18.5666666669527,-1.7320508079979));
#6830=CARTESIAN_POINT('Ctrl Pts',(2.00000000049539,18.5083333336194,-1.15470053866527));
#6831=CARTESIAN_POINT('Ctrl Pts',(2.00000000049539,18.450000000286,-2.44929359890139E-16));
#6832=CARTESIAN_POINT('Ctrl Pts',(2.00000000049539,18.3916666669527,1.15470053866527));
#6833=CARTESIAN_POINT('Ctrl Pts',(1.0000000002477,18.3333333336194,1.7320508079979));
#6834=CARTESIAN_POINT('Ctrl Pts',(4.24230095595043E-16,18.275000000286,
2.30940107733053));
#6835=CARTESIAN_POINT('Ctrl Pts',(-1.0000000002477,18.2166666669527,1.7320508079979));
#6836=CARTESIAN_POINT('Ctrl Pts',(-2.00000000049539,18.1583333336194,1.15470053866527));
#6837=CARTESIAN_POINT('Ctrl Pts',(-2.00000000049539,18.100000000286,0.));
#6838=CARTESIAN_POINT('Ctrl Pts',(-2.00000000049539,18.0416666669527,-1.15470053866527));
#6839=CARTESIAN_POINT('Ctrl Pts',(-1.0000000002477,17.9833333336194,-1.7320508079979));
#6840=CARTESIAN_POINT('Ctrl Pts',(-1.41410031865014E-16,17.925000000286,
-2.30940107733053));
#6841=CARTESIAN_POINT('Ctrl Pts',(1.0000000002477,17.8666666669527,-1.7320508079979));
#6842=CARTESIAN_POINT('Ctrl Pts',(2.00000000049539,17.8083333336194,-1.15470053866527));
#6843=CARTESIAN_POINT('Ctrl Pts',(2.00000000049539,17.750000000286,-2.44929359890139E-16));
#6844=CARTESIAN_POINT('Ctrl Pts',(2.00000000049539,17.6916666669527,1.15470053866527));
#6845=CARTESIAN_POINT('Ctrl Pts',(1.0000000002477,17.6333333336194,1.7320508079979));
#6846=CARTESIAN_POINT('Ctrl Pts',(4.24230095595043E-16,17.575000000286,
2.30940107733053));
#6847=CARTESIAN_POINT('Ctrl Pts',(-1.0000000002477,17.5166666669527,1.7320508079979));
#6848=CARTESIAN_POINT('Ctrl Pts',(-2.00000000049539,17.4583333336194,1.15470053866527));
#6849=CARTESIAN_POINT('Ctrl Pts',(-2.00000000049539,17.400000000286,0.));
#6850=CARTESIAN_POINT('Ctrl Pts',(-2.00000000049539,17.3416666669527,-1.15470053866527));
#6851=CARTESIAN_POINT('Ctrl Pts',(-1.0000000002477,17.2833333336194,-1.7320508079979));
#6852=CARTESIAN_POINT('Ctrl Pts',(-1.41410031865014E-16,17.225000000286,
-2.30940107733053));
#6853=CARTESIAN_POINT('Ctrl Pts',(1.0000000002477,17.1666666669527,-1.7320508079979));
#6854=CARTESIAN_POINT('Ctrl Pts',(2.00000000049539,17.1083333336194,-1.15470053866527));
#6855=CARTESIAN_POINT('Ctrl Pts',(2.00000000049539,17.050000000286,-2.44929359890139E-16));
#6856=CARTESIAN_POINT('Ctrl Pts',(2.00000000049539,16.9916666669527,1.15470053866527));
#6857=CARTESIAN_POINT('Ctrl Pts',(1.0000000002477,16.9333333336194,1.7320508079979));
#6858=CARTESIAN_POINT('Ctrl Pts',(4.24230095595043E-16,16.875000000286,
2.30940107733053));
#6859=CARTESIAN_POINT('Ctrl Pts',(-1.0000000002477,16.8166666669527,1.7320508079979));
#6860=CARTESIAN_POINT('Ctrl Pts',(-2.00000000049539,16.7583333336194,1.15470053866527));
#6861=CARTESIAN_POINT('Ctrl Pts',(-2.00000000049539,16.700000000286,0.));
#6862=CARTESIAN_POINT('Ctrl Pts',(-2.00000000049539,16.6416666669527,-1.15470053866527));
#6863=CARTESIAN_POINT('Ctrl Pts',(-1.0000000002477,16.5833333336194,-1.7320508079979));
#6864=CARTESIAN_POINT('Ctrl Pts',(-1.41410031865014E-16,16.525000000286,
-2.30940107733053));
#6865=CARTESIAN_POINT('Ctrl Pts',(1.0000000002477,16.4666666669527,-1.7320508079979));
#6866=CARTESIAN_POINT('Ctrl Pts',(2.00000000049539,16.4083333336194,-1.15470053866527));
#6867=CARTESIAN_POINT('Ctrl Pts',(2.00000000049539,16.350000000286,-2.44929359890139E-16));
#6868=CARTESIAN_POINT('Ctrl Pts',(2.00000000049539,16.2916666669527,1.15470053866527));
#6869=CARTESIAN_POINT('Ctrl Pts',(1.0000000002477,16.2333333336194,1.7320508079979));
#6870=CARTESIAN_POINT('Ctrl Pts',(4.24230095595043E-16,16.175000000286,
2.30940107733053));
#6871=CARTESIAN_POINT('Ctrl Pts',(-1.0000000002477,16.1166666669527,1.7320508079979));
#6872=CARTESIAN_POINT('Ctrl Pts',(-2.00000000049539,16.0583333336194,1.15470053866527));
#6873=CARTESIAN_POINT('Ctrl Pts',(-2.00000000049539,16.000000000286,0.));
#6874=CARTESIAN_POINT('Ctrl Pts',(-2.00000000049539,15.9416666669527,-1.15470053866527));
#6875=CARTESIAN_POINT('Ctrl Pts',(-1.0000000002477,15.8833333336194,-1.7320508079979));
#6876=CARTESIAN_POINT('Ctrl Pts',(-1.41410031865014E-16,15.825000000286,
-2.30940107733053));
#6877=CARTESIAN_POINT('Ctrl Pts',(1.0000000002477,15.7666666669527,-1.7320508079979));
#6878=CARTESIAN_POINT('Ctrl Pts',(2.00000000049539,15.7083333336194,-1.15470053866527));
#6879=CARTESIAN_POINT('Ctrl Pts',(2.00000000049539,15.650000000286,-2.44929359890139E-16));
#6880=CARTESIAN_POINT('Ctrl Pts',(2.00000000049539,15.5916666669527,1.15470053866527));
#6881=CARTESIAN_POINT('Ctrl Pts',(1.0000000002477,15.5333333336194,1.7320508079979));
#6882=CARTESIAN_POINT('Ctrl Pts',(4.24230095595043E-16,15.475000000286,
2.30940107733053));
#6883=CARTESIAN_POINT('Ctrl Pts',(-1.0000000002477,15.4166666669527,1.7320508079979));
#6884=CARTESIAN_POINT('Ctrl Pts',(-2.00000000049539,15.3583333336194,1.15470053866527));
#6885=CARTESIAN_POINT('Ctrl Pts',(-2.00000000049539,15.300000000286,0.));
#6886=CARTESIAN_POINT('Ctrl Pts',(-2.00000000049539,15.2416666669527,-1.15470053866527));
#6887=CARTESIAN_POINT('Ctrl Pts',(-1.0000000002477,15.1833333336194,-1.7320508079979));
#6888=CARTESIAN_POINT('Ctrl Pts',(-1.41410031865014E-16,15.125000000286,
-2.30940107733053));
#6889=CARTESIAN_POINT('Ctrl Pts',(1.0000000002477,15.0666666669527,-1.7320508079979));
#6890=CARTESIAN_POINT('Ctrl Pts',(2.00000000049539,15.0083333336194,-1.15470053866527));
#6891=CARTESIAN_POINT('Ctrl Pts',(2.00000000049539,14.950000000286,-2.44929359890139E-16));
#6892=CARTESIAN_POINT('Ctrl Pts',(2.00000000049539,14.8916666669527,1.15470053866527));
#6893=CARTESIAN_POINT('Ctrl Pts',(1.0000000002477,14.8333333336194,1.7320508079979));
#6894=CARTESIAN_POINT('Ctrl Pts',(4.24230095595043E-16,14.775000000286,
2.30940107733053));
#6895=CARTESIAN_POINT('Ctrl Pts',(-1.0000000002477,14.7166666669527,1.7320508079979));
#6896=CARTESIAN_POINT('Ctrl Pts',(-2.00000000049539,14.6583333336194,1.15470053866527));
#6897=CARTESIAN_POINT('Ctrl Pts',(-2.00000000049539,14.600000000286,0.));
#6898=CARTESIAN_POINT('Ctrl Pts',(-2.00000000049539,14.5416666669527,-1.15470053866527));
#6899=CARTESIAN_POINT('Ctrl Pts',(-1.0000000002477,14.4833333336194,-1.7320508079979));
#6900=CARTESIAN_POINT('Ctrl Pts',(-1.41410031865014E-16,14.425000000286,
-2.30940107733053));
#6901=CARTESIAN_POINT('Ctrl Pts',(1.0000000002477,14.3666666669527,-1.7320508079979));
#6902=CARTESIAN_POINT('Ctrl Pts',(2.00000000049539,14.3083333336194,-1.15470053866527));
#6903=CARTESIAN_POINT('Ctrl Pts',(2.00000000049539,14.250000000286,-2.44929359890139E-16));
#6904=CARTESIAN_POINT('Ctrl Pts',(2.00000000049539,14.1916666669527,1.15470053866527));
#6905=CARTESIAN_POINT('Ctrl Pts',(1.0000000002477,14.1333333336194,1.7320508079979));
#6906=CARTESIAN_POINT('Ctrl Pts',(4.24230095595043E-16,14.075000000286,
2.30940107733053));
#6907=CARTESIAN_POINT('Ctrl Pts',(-1.0000000002477,14.0166666669527,1.7320508079979));
#6908=CARTESIAN_POINT('Ctrl Pts',(-2.00000000049539,13.9583333336194,1.15470053866527));
#6909=CARTESIAN_POINT('Ctrl Pts',(-2.00000000049539,13.900000000286,0.));
#6910=CARTESIAN_POINT('Ctrl Pts',(-2.00000000049539,13.8416666669527,-1.15470053866527));
#6911=CARTESIAN_POINT('Ctrl Pts',(-1.0000000002477,13.7833333336194,-1.7320508079979));
#6912=CARTESIAN_POINT('Ctrl Pts',(-1.41410031865014E-16,13.725000000286,
-2.30940107733053));
#6913=CARTESIAN_POINT('Ctrl Pts',(1.0000000002477,13.6666666669527,-1.7320508079979));
#6914=CARTESIAN_POINT('Ctrl Pts',(2.00000000049539,13.6083333336194,-1.15470053866527));
#6915=CARTESIAN_POINT('Ctrl Pts',(2.00000000049539,13.550000000286,-2.44929359890139E-16));
#6916=CARTESIAN_POINT('Ctrl Pts',(2.00000000049539,13.4916666669527,1.15470053866527));
#6917=CARTESIAN_POINT('Ctrl Pts',(1.0000000002477,13.4333333336194,1.7320508079979));
#6918=CARTESIAN_POINT('Ctrl Pts',(4.24230095595043E-16,13.375000000286,
2.30940107733053));
#6919=CARTESIAN_POINT('Ctrl Pts',(-1.0000000002477,13.3166666669527,1.7320508079979));
#6920=CARTESIAN_POINT('Ctrl Pts',(-2.00000000049539,13.2583333336194,1.15470053866527));
#6921=CARTESIAN_POINT('Ctrl Pts',(-2.00000000049539,13.200000000286,0.));
#6922=CARTESIAN_POINT('Ctrl Pts',(-2.00000000049539,13.1416666669527,-1.15470053866527));
#6923=CARTESIAN_POINT('Ctrl Pts',(-1.0000000002477,13.0833333336194,-1.7320508079979));
#6924=CARTESIAN_POINT('Ctrl Pts',(-1.41410031865014E-16,13.025000000286,
-2.30940107733053));
#6925=CARTESIAN_POINT('Ctrl Pts',(1.0000000002477,12.9666666669527,-1.7320508079979));
#6926=CARTESIAN_POINT('Ctrl Pts',(2.00000000049539,12.9083333336194,-1.15470053866527));
#6927=CARTESIAN_POINT('Ctrl Pts',(2.00000000049539,12.850000000286,-2.44929359890139E-16));
#6928=CARTESIAN_POINT('Ctrl Pts',(2.00000000049539,12.7916666669527,1.15470053866527));
#6929=CARTESIAN_POINT('Ctrl Pts',(1.0000000002477,12.7333333336194,1.7320508079979));
#6930=CARTESIAN_POINT('Ctrl Pts',(4.24230095595043E-16,12.675000000286,
2.30940107733053));
#6931=CARTESIAN_POINT('Ctrl Pts',(-1.0000000002477,12.6166666669527,1.7320508079979));
#6932=CARTESIAN_POINT('Ctrl Pts',(-2.00000000049539,12.5583333336194,1.15470053866527));
#6933=CARTESIAN_POINT('Ctrl Pts',(-2.00000000049539,12.500000000286,0.));
#6934=CARTESIAN_POINT('Ctrl Pts',(-2.00000000049539,12.4416666669527,-1.15470053866527));
#6935=CARTESIAN_POINT('Ctrl Pts',(-1.0000000002477,12.3833333336194,-1.7320508079979));
#6936=CARTESIAN_POINT('Ctrl Pts',(-1.41410031865014E-16,12.325000000286,
-2.30940107733053));
#6937=CARTESIAN_POINT('Ctrl Pts',(1.0000000002477,12.2666666669527,-1.7320508079979));
#6938=CARTESIAN_POINT('Ctrl Pts',(2.00000000049539,12.2083333336194,-1.15470053866527));
#6939=CARTESIAN_POINT('Ctrl Pts',(2.00000000049539,12.150000000286,-2.44929359890139E-16));
#6940=CARTESIAN_POINT('Ctrl Pts',(2.00000000049539,12.0916666669527,1.15470053866527));
#6941=CARTESIAN_POINT('Ctrl Pts',(1.0000000002477,12.0333333336194,1.7320508079979));
#6942=CARTESIAN_POINT('Ctrl Pts',(4.24230095595043E-16,11.975000000286,
2.30940107733053));
#6943=CARTESIAN_POINT('Ctrl Pts',(-1.0000000002477,11.9166666669527,1.7320508079979));
#6944=CARTESIAN_POINT('Ctrl Pts',(-2.00000000049539,11.8583333336194,1.15470053866527));
#6945=CARTESIAN_POINT('Ctrl Pts',(-2.00000000049539,11.800000000286,0.));
#6946=CARTESIAN_POINT('Ctrl Pts',(-2.00000000049539,11.7416666669527,-1.15470053866527));
#6947=CARTESIAN_POINT('Ctrl Pts',(-1.0000000002477,11.6833333336194,-1.7320508079979));
#6948=CARTESIAN_POINT('Ctrl Pts',(-1.41410031865014E-16,11.625000000286,
-2.30940107733053));
#6949=CARTESIAN_POINT('Ctrl Pts',(1.0000000002477,11.5666666669527,-1.7320508079979));
#6950=CARTESIAN_POINT('Ctrl Pts',(2.00000000049539,11.5083333336194,-1.15470053866527));
#6951=CARTESIAN_POINT('Ctrl Pts',(2.00000000049539,11.450000000286,-2.44929359890139E-16));
#6952=CARTESIAN_POINT('Ctrl Pts',(2.00000000049539,11.3916666669527,1.15470053866527));
#6953=CARTESIAN_POINT('Ctrl Pts',(1.0000000002477,11.3333333336194,1.7320508079979));
#6954=CARTESIAN_POINT('Ctrl Pts',(4.24230095595043E-16,11.275000000286,
2.30940107733053));
#6955=CARTESIAN_POINT('Ctrl Pts',(-1.0000000002477,11.2166666669527,1.7320508079979));
#6956=CARTESIAN_POINT('Ctrl Pts',(-2.00000000049539,11.1583333336194,1.15470053866527));
#6957=CARTESIAN_POINT('Ctrl Pts',(-2.00000000049539,11.100000000286,0.));
#6958=CARTESIAN_POINT('Ctrl Pts',(-2.00000000049539,11.0416666669527,-1.15470053866527));
#6959=CARTESIAN_POINT('Ctrl Pts',(-1.0000000002477,10.9833333336194,-1.7320508079979));
#6960=CARTESIAN_POINT('Ctrl Pts',(-1.41410031865014E-16,10.925000000286,
-2.30940107733053));
#6961=CARTESIAN_POINT('Ctrl Pts',(1.0000000002477,10.8666666669527,-1.7320508079979));
#6962=CARTESIAN_POINT('Ctrl Pts',(2.00000000049539,10.8083333336194,-1.15470053866527));
#6963=CARTESIAN_POINT('Ctrl Pts',(2.00000000049539,10.750000000286,-2.44929359890139E-16));
#6964=CARTESIAN_POINT('Ctrl Pts',(2.00000000049539,10.6916666669527,1.15470053866527));
#6965=CARTESIAN_POINT('Ctrl Pts',(1.0000000002477,10.6333333336194,1.7320508079979));
#6966=CARTESIAN_POINT('Ctrl Pts',(4.24230095595043E-16,10.575000000286,
2.30940107733053));
#6967=CARTESIAN_POINT('Ctrl Pts',(-1.0000000002477,10.5166666669527,1.7320508079979));
#6968=CARTESIAN_POINT('Ctrl Pts',(-2.00000000049539,10.4583333336194,1.15470053866527));
#6969=CARTESIAN_POINT('Ctrl Pts',(-2.00000000049539,10.400000000286,0.));
#6970=CARTESIAN_POINT('Ctrl Pts',(-2.00000000049539,10.3416666669527,-1.15470053866527));
#6971=CARTESIAN_POINT('Ctrl Pts',(-1.0000000002477,10.2833333336194,-1.7320508079979));
#6972=CARTESIAN_POINT('Ctrl Pts',(-1.41410031865014E-16,10.225000000286,
-2.30940107733053));
#6973=CARTESIAN_POINT('Ctrl Pts',(1.0000000002477,10.1666666669527,-1.7320508079979));
#6974=CARTESIAN_POINT('Ctrl Pts',(2.00000000049539,10.1083333336194,-1.15470053866527));
#6975=CARTESIAN_POINT('Ctrl Pts',(2.00000000049539,10.050000000286,-2.44929359890139E-16));
#6976=CARTESIAN_POINT('Ctrl Pts',(2.00000000049539,9.99166666695269,1.15470053866527));
#6977=CARTESIAN_POINT('Ctrl Pts',(1.0000000002477,9.93333333361936,1.7320508079979));
#6978=CARTESIAN_POINT('Ctrl Pts',(4.24230095595043E-16,9.87500000028603,
2.30940107733053));
#6979=CARTESIAN_POINT('Ctrl Pts',(-1.0000000002477,9.81666666695269,1.7320508079979));
#6980=CARTESIAN_POINT('Ctrl Pts',(-2.00000000049539,9.75833333361936,1.15470053866527));
#6981=CARTESIAN_POINT('Ctrl Pts',(-2.00000000049539,9.70000000028602,0.));
#6982=CARTESIAN_POINT('Ctrl Pts',(-2.00000000049539,9.64166666695269,-1.15470053866527));
#6983=CARTESIAN_POINT('Ctrl Pts',(-1.0000000002477,9.58333333361935,-1.7320508079979));
#6984=CARTESIAN_POINT('Ctrl Pts',(-1.41410031865014E-16,9.52500000028602,
-2.30940107733053));
#6985=CARTESIAN_POINT('Ctrl Pts',(1.0000000002477,9.4666666669527,-1.7320508079979));
#6986=CARTESIAN_POINT('Ctrl Pts',(2.00000000049539,9.40833333361935,-1.15470053866527));
#6987=CARTESIAN_POINT('Ctrl Pts',(2.00000000049539,9.35000000028603,-2.44929359890139E-16));
#6988=CARTESIAN_POINT('Ctrl Pts',(2.00000000049539,9.29166666695269,1.15470053866527));
#6989=CARTESIAN_POINT('Ctrl Pts',(1.0000000002477,9.23333333361936,1.7320508079979));
#6990=CARTESIAN_POINT('Ctrl Pts',(4.24230095595043E-16,9.17500000028602,
2.30940107733053));
#6991=CARTESIAN_POINT('Ctrl Pts',(-1.0000000002477,9.11666666695269,1.7320508079979));
#6992=CARTESIAN_POINT('Ctrl Pts',(-2.00000000049539,9.05833333361936,1.15470053866527));
#6993=CARTESIAN_POINT('Ctrl Pts',(-2.00000000049539,9.00000000028602,0.));
#6994=CARTESIAN_POINT('Ctrl Pts',(-2.00000000049539,8.9416666669527,-1.15470053866527));
#6995=CARTESIAN_POINT('Ctrl Pts',(-1.0000000002477,8.88333333361936,-1.7320508079979));
#6996=CARTESIAN_POINT('Ctrl Pts',(-1.41410031865014E-16,8.82500000028603,
-2.30940107733053));
#6997=CARTESIAN_POINT('Ctrl Pts',(1.0000000002477,8.76666666695269,-1.7320508079979));
#6998=CARTESIAN_POINT('Ctrl Pts',(2.00000000049539,8.70833333361936,-1.15470053866527));
#6999=CARTESIAN_POINT('Ctrl Pts',(2.00000000049539,8.65000000028602,-2.44929359890139E-16));
#7000=CARTESIAN_POINT('Ctrl Pts',(2.00000000049539,8.59166666695269,1.15470053866527));
#7001=CARTESIAN_POINT('Ctrl Pts',(1.0000000002477,8.53333333361935,1.7320508079979));
#7002=CARTESIAN_POINT('Ctrl Pts',(4.24230095595043E-16,8.47500000028603,
2.30940107733053));
#7003=CARTESIAN_POINT('Ctrl Pts',(-1.0000000002477,8.41666666695269,1.7320508079979));
#7004=CARTESIAN_POINT('Ctrl Pts',(-2.00000000049539,8.35833333361936,1.15470053866527));
#7005=CARTESIAN_POINT('Ctrl Pts',(-2.00000000049539,8.30000000028603,0.));
#7006=CARTESIAN_POINT('Ctrl Pts',(-2.00000000049539,8.24166666695269,-1.15470053866527));
#7007=CARTESIAN_POINT('Ctrl Pts',(-1.0000000002477,8.18333333361936,-1.7320508079979));
#7008=CARTESIAN_POINT('Ctrl Pts',(-1.41410031865014E-16,8.12500000028602,
-2.30940107733053));
#7009=CARTESIAN_POINT('Ctrl Pts',(1.0000000002477,8.0666666669527,-1.7320508079979));
#7010=CARTESIAN_POINT('Ctrl Pts',(2.00000000049539,8.00833333361936,-1.15470053866527));
#7011=CARTESIAN_POINT('Ctrl Pts',(2.00000000049539,7.95000000028603,-2.44929359890139E-16));
#7012=CARTESIAN_POINT('Ctrl Pts',(2.00000000049539,7.89166666695269,1.15470053866527));
#7013=CARTESIAN_POINT('Ctrl Pts',(1.0000000002477,7.83333333361936,1.7320508079979));
#7014=CARTESIAN_POINT('Ctrl Pts',(4.24230095595043E-16,7.77500000028602,
2.30940107733053));
#7015=CARTESIAN_POINT('Ctrl Pts',(-1.0000000002477,7.71666666695269,1.7320508079979));
#7016=CARTESIAN_POINT('Ctrl Pts',(-2.00000000049539,7.65833333361935,1.15470053866527));
#7017=CARTESIAN_POINT('Ctrl Pts',(-2.00000000049539,7.60000000028603,0.));
#7018=CARTESIAN_POINT('Ctrl Pts',(-2.00000000049539,7.5416666669527,-1.15470053866527));
#7019=CARTESIAN_POINT('Ctrl Pts',(-1.0000000002477,7.48333333361936,-1.7320508079979));
#7020=CARTESIAN_POINT('Ctrl Pts',(-1.41410031865014E-16,7.42500000028603,
-2.30940107733053));
#7021=CARTESIAN_POINT('Ctrl Pts',(1.0000000002477,7.36666666695269,-1.7320508079979));
#7022=CARTESIAN_POINT('Ctrl Pts',(2.00000000049539,7.30833333361936,-1.15470053866527));
#7023=CARTESIAN_POINT('Ctrl Pts',(2.00000000049539,7.25000000028602,-2.44929359890139E-16));
#7024=CARTESIAN_POINT('Ctrl Pts',(2.00000000049539,7.1916666669527,1.15470053866527));
#7025=CARTESIAN_POINT('Ctrl Pts',(1.0000000002477,7.13333333361935,1.7320508079979));
#7026=CARTESIAN_POINT('Ctrl Pts',(4.24230095595043E-16,7.07500000028603,
2.30940107733053));
#7027=CARTESIAN_POINT('Ctrl Pts',(-1.0000000002477,7.01666666695269,1.7320508079979));
#7028=CARTESIAN_POINT('Ctrl Pts',(-2.00000000049539,6.95833333361936,1.15470053866527));
#7029=CARTESIAN_POINT('Ctrl Pts',(-2.00000000049539,6.90000000028602,0.));
#7030=CARTESIAN_POINT('Ctrl Pts',(-2.00000000049539,6.84166666695269,-1.15470053866527));
#7031=CARTESIAN_POINT('Ctrl Pts',(-1.0000000002477,6.78333333361935,-1.7320508079979));
#7032=CARTESIAN_POINT('Ctrl Pts',(-1.41410031865014E-16,6.72500000028603,
-2.30940107733053));
#7033=CARTESIAN_POINT('Ctrl Pts',(1.0000000002477,6.6666666669527,-1.7320508079979));
#7034=CARTESIAN_POINT('Ctrl Pts',(2.00000000049539,6.60833333361936,-1.15470053866527));
#7035=CARTESIAN_POINT('Ctrl Pts',(2.00000000049539,6.55000000028603,-2.44929359890139E-16));
#7036=CARTESIAN_POINT('Ctrl Pts',(2.00000000049539,6.49166666695269,1.15470053866527));
#7037=CARTESIAN_POINT('Ctrl Pts',(1.0000000002477,6.43333333361936,1.7320508079979));
#7038=CARTESIAN_POINT('Ctrl Pts',(4.24230095595043E-16,6.37500000028602,
2.30940107733053));
#7039=CARTESIAN_POINT('Ctrl Pts',(-1.0000000002477,6.31666666695269,1.7320508079979));
#7040=CARTESIAN_POINT('Ctrl Pts',(-2.00000000049539,6.25833333361935,1.15470053866527));
#7041=CARTESIAN_POINT('Ctrl Pts',(-2.00000000049539,6.20000000028603,0.));
#7042=CARTESIAN_POINT('Ctrl Pts',(-2.00000000049539,6.14166666695269,-1.15470053866527));
#7043=CARTESIAN_POINT('Ctrl Pts',(-1.0000000002477,6.08333333361936,-1.7320508079979));
#7044=CARTESIAN_POINT('Ctrl Pts',(-1.41410031865014E-16,6.02500000028602,
-2.30940107733053));
#7045=CARTESIAN_POINT('Ctrl Pts',(1.0000000002477,5.96666666695269,-1.7320508079979));
#7046=CARTESIAN_POINT('Ctrl Pts',(2.00000000049539,5.90833333361937,-1.15470053866527));
#7047=CARTESIAN_POINT('Ctrl Pts',(2.00000000049539,5.85000000028602,-2.44929359890139E-16));
#7048=CARTESIAN_POINT('Ctrl Pts',(2.00000000049539,5.7916666669527,1.15470053866527));
#7049=CARTESIAN_POINT('Ctrl Pts',(1.0000000002477,5.73333333361935,1.7320508079979));
#7050=CARTESIAN_POINT('Ctrl Pts',(4.24230095595043E-16,5.67500000028603,
2.30940107733053));
#7051=CARTESIAN_POINT('Ctrl Pts',(-1.0000000002477,5.61666666695269,1.7320508079979));
#7052=CARTESIAN_POINT('Ctrl Pts',(-2.00000000049539,5.55833333361936,1.15470053866527));
#7053=CARTESIAN_POINT('Ctrl Pts',(-2.00000000049539,5.50000000028602,0.));
#7054=CARTESIAN_POINT('Ctrl Pts',(-2.00000000049539,5.44166666695269,-1.15470053866527));
#7055=CARTESIAN_POINT('Ctrl Pts',(-1.0000000002477,5.38333333361935,-1.7320508079979));
#7056=CARTESIAN_POINT('Ctrl Pts',(-1.41410031865014E-16,5.32500000028603,
-2.30940107733053));
#7057=CARTESIAN_POINT('Ctrl Pts',(1.0000000002477,5.26666666695268,-1.7320508079979));
#7058=CARTESIAN_POINT('Ctrl Pts',(2.00000000049539,5.20833333361936,-1.15470053866527));
#7059=CARTESIAN_POINT('Ctrl Pts',(2.00000000049539,5.15000000028603,-2.44929359890139E-16));
#7060=CARTESIAN_POINT('Ctrl Pts',(2.00000000049539,5.09166666695269,1.15470053866527));
#7061=CARTESIAN_POINT('Ctrl Pts',(1.0000000002477,5.03333333361936,1.7320508079979));
#7062=CARTESIAN_POINT('Ctrl Pts',(4.24230095595043E-16,4.97500000028602,
2.30940107733053));
#7063=CARTESIAN_POINT('Ctrl Pts',(-1.0000000002477,4.9166666669527,1.7320508079979));
#7064=CARTESIAN_POINT('Ctrl Pts',(-2.00000000049539,4.85833333361936,1.15470053866527));
#7065=CARTESIAN_POINT('Ctrl Pts',(-2.00000000049539,4.80000000028603,0.));
#7066=CARTESIAN_POINT('Ctrl Pts',(-2.00000000049539,4.74166666695269,-1.15470053866527));
#7067=CARTESIAN_POINT('Ctrl Pts',(-1.0000000002477,4.68333333361936,-1.7320508079979));
#7068=CARTESIAN_POINT('Ctrl Pts',(-1.41410031865014E-16,4.62500000028602,
-2.30940107733053));
#7069=CARTESIAN_POINT('Ctrl Pts',(1.0000000002477,4.56666666695269,-1.7320508079979));
#7070=CARTESIAN_POINT('Ctrl Pts',(2.00000000049539,4.50833333361935,-1.15470053866527));
#7071=CARTESIAN_POINT('Ctrl Pts',(2.00000000049539,4.45000000028603,-2.44929359890139E-16));
#7072=CARTESIAN_POINT('Ctrl Pts',(2.00000000049539,4.3916666669527,1.15470053866527));
#7073=CARTESIAN_POINT('Ctrl Pts',(1.0000000002477,4.33333333361936,1.7320508079979));
#7074=CARTESIAN_POINT('Ctrl Pts',(4.24230095595043E-16,4.27500000028603,
2.30940107733053));
#7075=CARTESIAN_POINT('Ctrl Pts',(-1.0000000002477,4.21666666695269,1.7320508079979));
#7076=CARTESIAN_POINT('Ctrl Pts',(-2.00000000049539,4.15833333361936,1.15470053866527));
#7077=CARTESIAN_POINT('Ctrl Pts',(-2.00000000049539,4.10000000028602,0.));
#7078=CARTESIAN_POINT('Ctrl Pts',(-2.00000000049539,4.0416666669527,-1.15470053866527));
#7079=CARTESIAN_POINT('Ctrl Pts',(-1.0000000002477,3.98333333361935,-1.7320508079979));
#7080=CARTESIAN_POINT('Ctrl Pts',(-1.41410031865014E-16,3.92500000028603,
-2.30940107733053));
#7081=CARTESIAN_POINT('Ctrl Pts',(1.0000000002477,3.86666666695269,-1.7320508079979));
#7082=CARTESIAN_POINT('Ctrl Pts',(2.00000000049539,3.80833333361936,-1.15470053866527));
#7083=CARTESIAN_POINT('Ctrl Pts',(2.00000000049539,3.75000000028602,-2.44929359890139E-16));
#7084=CARTESIAN_POINT('Ctrl Pts',(2.00000000049539,3.69166666695269,1.15470053866527));
#7085=CARTESIAN_POINT('Ctrl Pts',(1.0000000002477,3.63333333361935,1.7320508079979));
#7086=CARTESIAN_POINT('Ctrl Pts',(4.24230095595043E-16,3.57500000028602,
2.30940107733053));
#7087=CARTESIAN_POINT('Ctrl Pts',(-1.0000000002477,3.5166666669527,1.7320508079979));
#7088=CARTESIAN_POINT('Ctrl Pts',(-2.00000000049539,3.45833333361936,1.15470053866527));
#7089=CARTESIAN_POINT('Ctrl Pts',(-2.00000000049539,3.40000000028603,0.));
#7090=CARTESIAN_POINT('Ctrl Pts',(-2.00000000049539,3.34166666695269,-1.15470053866527));
#7091=CARTESIAN_POINT('Ctrl Pts',(-1.0000000002477,3.28333333361936,-1.7320508079979));
#7092=CARTESIAN_POINT('Ctrl Pts',(-1.41410031865014E-16,3.22500000028602,
-2.30940107733053));
#7093=CARTESIAN_POINT('Ctrl Pts',(1.0000000002477,3.16666666695269,-1.7320508079979));
#7094=CARTESIAN_POINT('Ctrl Pts',(2.00000000049539,3.10833333361935,-1.15470053866527));
#7095=CARTESIAN_POINT('Ctrl Pts',(2.00000000049539,3.05000000028603,-2.44929359890139E-16));
#7096=CARTESIAN_POINT('Ctrl Pts',(2.00000000049539,2.99166666695269,1.15470053866527));
#7097=CARTESIAN_POINT('Ctrl Pts',(1.0000000002477,2.93333333361936,1.7320508079979));
#7098=CARTESIAN_POINT('Ctrl Pts',(4.24230095595043E-16,2.87500000028602,
2.30940107733053));
#7099=CARTESIAN_POINT('Ctrl Pts',(-1.0000000002477,2.81666666695269,1.7320508079979));
#7100=CARTESIAN_POINT('Ctrl Pts',(-2.00000000049539,2.75833333361936,1.15470053866527));
#7101=CARTESIAN_POINT('Ctrl Pts',(-2.00000000049539,2.70000000028602,0.));
#7102=CARTESIAN_POINT('Ctrl Pts',(-2.00000000049539,2.6416666669527,-1.15470053866527));
#7103=CARTESIAN_POINT('Ctrl Pts',(-1.0000000002477,2.58333333361936,-1.7320508079979));
#7104=CARTESIAN_POINT('Ctrl Pts',(-1.41410031865014E-16,2.52500000028603,
-2.30940107733053));
#7105=CARTESIAN_POINT('Ctrl Pts',(1.0000000002477,2.46666666695269,-1.7320508079979));
#7106=CARTESIAN_POINT('Ctrl Pts',(2.00000000049539,2.40833333361936,-1.15470053866527));
#7107=CARTESIAN_POINT('Ctrl Pts',(2.00000000049539,2.35000000028602,-2.44929359890139E-16));
#7108=CARTESIAN_POINT('Ctrl Pts',(2.00000000049539,2.29166666695269,1.15470053866527));
#7109=CARTESIAN_POINT('Ctrl Pts',(1.0000000002477,2.23333333361935,1.7320508079979));
#7110=CARTESIAN_POINT('Ctrl Pts',(4.24230095595043E-16,2.17500000028603,
2.30940107733053));
#7111=CARTESIAN_POINT('Ctrl Pts',(-1.0000000002477,2.11666666695269,1.7320508079979));
#7112=CARTESIAN_POINT('Ctrl Pts',(-2.00000000049539,2.05833333361936,1.15470053866527));
#7113=CARTESIAN_POINT('Ctrl Pts',(-2.00000000049539,2.00000000028603,0.));
#7114=CARTESIAN_POINT('Ctrl Pts',(-2.00000000049539,1.94166666695269,-1.15470053866527));
#7115=CARTESIAN_POINT('Ctrl Pts',(-1.0000000002477,1.88333333361936,-1.7320508079979));
#7116=CARTESIAN_POINT('Ctrl Pts',(-1.41410031865014E-16,1.82500000028602,
-2.30940107733053));
#7117=CARTESIAN_POINT('Ctrl Pts',(1.0000000002477,1.7666666669527,-1.7320508079979));
#7118=CARTESIAN_POINT('Ctrl Pts',(2.00000000049539,1.70833333361935,-1.15470053866527));
#7119=CARTESIAN_POINT('Ctrl Pts',(2.00000000049539,1.65000000028603,-2.44929359890139E-16));
#7120=CARTESIAN_POINT('Ctrl Pts',(2.00000000049539,1.59166666695269,1.15470053866527));
#7121=CARTESIAN_POINT('Ctrl Pts',(1.0000000002477,1.53333333361936,1.7320508079979));
#7122=CARTESIAN_POINT('Ctrl Pts',(4.24230095595043E-16,1.47500000028602,
2.30940107733053));
#7123=CARTESIAN_POINT('Ctrl Pts',(-1.0000000002477,1.41666666695269,1.7320508079979));
#7124=CARTESIAN_POINT('Ctrl Pts',(-2.00000000049539,1.35833333361935,1.15470053866527));
#7125=CARTESIAN_POINT('Ctrl Pts',(-2.00000000049539,1.30000000028603,0.));
#7126=CARTESIAN_POINT('Ctrl Pts',(-2.00000000049539,1.2416666669527,-1.15470053866527));
#7127=CARTESIAN_POINT('Ctrl Pts',(-1.0000000002477,1.18333333361936,-1.7320508079979));
#7128=CARTESIAN_POINT('Ctrl Pts',(-1.41410031865014E-16,1.12500000028603,
-2.30940107733053));
#7129=CARTESIAN_POINT('Ctrl Pts',(1.0000000002477,1.06666666695269,-1.7320508079979));
#7130=CARTESIAN_POINT('Ctrl Pts',(2.00000000049539,1.00833333361936,-1.15470053866527));
#7131=CARTESIAN_POINT('Ctrl Pts',(2.00000000049539,0.950000000286022,-2.44929359890139E-16));
#7132=CARTESIAN_POINT('Ctrl Pts',(2.00000000049539,0.891666666952695,1.15470053866527));
#7133=CARTESIAN_POINT('Ctrl Pts',(1.0000000002477,0.833333333619354,1.7320508079979));
#7134=CARTESIAN_POINT('Ctrl Pts',(4.24230095595043E-16,0.775000000286027,
2.30940107733053));
#7135=CARTESIAN_POINT('Ctrl Pts',(-1.0000000002477,0.716666666952686,1.7320508079979));
#7136=CARTESIAN_POINT('Ctrl Pts',(-2.00000000049539,0.65833333361936,1.15470053866527));
#7137=CARTESIAN_POINT('Ctrl Pts',(-2.00000000049539,0.600000000286019,0.));
#7138=CARTESIAN_POINT('Ctrl Pts',(-2.00000000049539,0.541666666952692,-1.15470053866527));
#7139=CARTESIAN_POINT('Ctrl Pts',(-1.0000000002477,0.483333333619351,-1.7320508079979));
#7140=CARTESIAN_POINT('Ctrl Pts',(-1.41410031865014E-16,0.425000000286024,
-2.30940107733053));
#7141=CARTESIAN_POINT('Ctrl Pts',(1.0000000002477,0.366666666952697,-1.7320508079979));
#7142=CARTESIAN_POINT('Ctrl Pts',(2.00000000049539,0.308333333619356,-1.15470053866527));
#7143=CARTESIAN_POINT('Ctrl Pts',(2.00000000049539,0.250000000286029,-2.44929359890139E-16));
#7144=CARTESIAN_POINT('Ctrl Pts',(2.00000000049539,0.191666666952689,1.15470053866527));
#7145=CARTESIAN_POINT('Ctrl Pts',(1.0000000002477,0.133333333619362,1.7320508079979));
#7146=CARTESIAN_POINT('Ctrl Pts',(4.24230095595043E-16,0.075000000286021,
2.30940107733053));
#7147=CARTESIAN_POINT('Ctrl Pts',(-1.0000000002477,0.0166666669526941,1.7320508079979));
#7148=CARTESIAN_POINT('Ctrl Pts',(-2.00000000049539,-0.0416666663806467,
1.15470053866527));
#7149=CARTESIAN_POINT('Ctrl Pts',(-2.00000000049539,-0.0999999997139736,
0.));
#7150=CARTESIAN_POINT('Ctrl Pts',(-2.00000000049539,-0.158333333047314,
-1.15470053866527));
#7151=CARTESIAN_POINT('Ctrl Pts',(-1.0000000002477,-0.216666666380641,-1.7320508079979));
#7152=CARTESIAN_POINT('Ctrl Pts',(-1.41410031865014E-16,-0.274999999713982,
-2.30940107733053));
#7153=CARTESIAN_POINT('Ctrl Pts',(1.0000000002477,-0.333333333047309,-1.7320508079979));
#7154=CARTESIAN_POINT('Ctrl Pts',(2.00000000049539,-0.391666666380636,-1.15470053866527));
#7155=CARTESIAN_POINT('Ctrl Pts',(2.00000000049539,-0.449999999713977,-2.44929359890139E-16));
#7156=CARTESIAN_POINT('Ctrl Pts',(2.00000000049539,-0.508333333047304,1.15470053866527));
#7157=CARTESIAN_POINT('Ctrl Pts',(1.0000000002477,-0.566666666380644,1.7320508079979));
#7158=CARTESIAN_POINT('Ctrl Pts',(4.24230095595043E-16,-0.624999999713971,
2.30940107733053));
#7159=CARTESIAN_POINT('Ctrl Pts',(-1.0000000002477,-0.683333333047312,1.7320508079979));
#7160=CARTESIAN_POINT('Ctrl Pts',(-2.00000000049539,-0.741666666380639,
1.15470053866527));
#7161=CARTESIAN_POINT('Ctrl Pts',(-2.00000000049539,-0.79999999971398,0.));
#7162=CARTESIAN_POINT('Ctrl Pts',(-2.00000000049539,-0.858333333047307,
-1.15470053866527));
#7163=CARTESIAN_POINT('Ctrl Pts',(-1.0000000002477,-0.916666666380648,-1.7320508079979));
#7164=CARTESIAN_POINT('Ctrl Pts',(-1.41410031865014E-16,-0.974999999713974,
-2.30940107733053));
#7165=CARTESIAN_POINT('Ctrl Pts',(1.0000000002477,-1.03333333304732,-1.7320508079979));
#7166=CARTESIAN_POINT('Ctrl Pts',(2.00000000049539,-1.09166666638064,-1.15470053866527));
#7167=CARTESIAN_POINT('Ctrl Pts',(2.00000000049539,-1.14999999971397,-2.44929359890139E-16));
#7168=CARTESIAN_POINT('Ctrl Pts',(2.00000000049539,-1.20833333304731,1.15470053866527));
#7169=CARTESIAN_POINT('Ctrl Pts',(1.0000000002477,-1.26666666638064,1.7320508079979));
#7170=CARTESIAN_POINT('Ctrl Pts',(4.24230095595043E-16,-1.32499999971398,
2.30940107733053));
#7171=CARTESIAN_POINT('Ctrl Pts',(-1.0000000002477,-1.3833333330473,1.7320508079979));
#7172=CARTESIAN_POINT('Ctrl Pts',(-2.00000000049539,-1.44166666638065,1.15470053866527));
#7173=CARTESIAN_POINT('Ctrl Pts',(-2.00000000049539,-1.49999999971397,0.));
#7174=CARTESIAN_POINT('Ctrl Pts',(-2.00000000049539,-1.55833333304731,-1.15470053866527));
#7175=CARTESIAN_POINT('Ctrl Pts',(-1.0000000002477,-1.61666666638064,-1.7320508079979));
#7176=CARTESIAN_POINT('Ctrl Pts',(-1.41410031865014E-16,-1.67499999971398,
-2.30940107733053));
#7177=CARTESIAN_POINT('Ctrl Pts',(1.0000000002477,-1.73333333304731,-1.7320508079979));
#7178=CARTESIAN_POINT('Ctrl Pts',(2.00000000049539,-1.79166666638065,-1.15470053866527));
#7179=CARTESIAN_POINT('Ctrl Pts',(2.00000000049539,-1.84999999971398,-2.44929359890139E-16));
#7180=CARTESIAN_POINT('Ctrl Pts',(2.00000000049539,-1.9083333330473,1.15470053866527));
#7181=CARTESIAN_POINT('Ctrl Pts',(1.0000000002477,-1.96666666638064,1.7320508079979));
#7182=CARTESIAN_POINT('Ctrl Pts',(0.738898696525379,-1.98189757576067,1.88279771598774));
#7183=CARTESIAN_POINT('Ctrl Pts',(0.444961184151523,-1.9990439306449,1.94987423865747));
#7184=CARTESIAN_POINT('Ctrl Pts',(-1.52006374725761,9.52000000000001,0.563397231550268));
#7185=CARTESIAN_POINT('Ctrl Pts',(-1.58927882503764,9.52000000000001,0.429537689746389));
#7186=CARTESIAN_POINT('Ctrl Pts',(-1.63814900638563,9.52000000000001,0.288940715437786));
#7187=CARTESIAN_POINT('Ctrl Pts',(-1.69591065797373,9.52000000000001,-0.00549261577426306));
#7188=CARTESIAN_POINT('Ctrl Pts',(-1.70375959008733,9.52000000000001,-0.15553028221414));
#7189=CARTESIAN_POINT('Ctrl Pts',(-1.68351521825398,9.52000000000001,-0.453449224894565));
#7190=CARTESIAN_POINT('Ctrl Pts',(-1.65426345691986,9.52,-0.602019915388218));
#7191=CARTESIAN_POINT('Ctrl Pts',(-1.56087360396711,9.52,-0.884017448979234));
#7192=CARTESIAN_POINT('Ctrl Pts',(-1.49537671531736,9.52000000000001,-1.02113231381166));
#7193=CARTESIAN_POINT('Ctrl Pts',(-1.3343529445858,9.52000000000001,-1.27139381246717));
#7194=CARTESIAN_POINT('Ctrl Pts',(-1.23864034261375,9.52000000000001,-1.3859272903417));
#7195=CARTESIAN_POINT('Ctrl Pts',(-1.01839953499697,9.52000000000001,-1.59036808297552));
#7196=CARTESIAN_POINT('Ctrl Pts',(-0.897345930978197,9.52000000000001,-1.67656690067514));
#7197=CARTESIAN_POINT('Ctrl Pts',(-0.636953702877006,9.52000000000001,-1.82216955557148));
#7198=CARTESIAN_POINT('Ctrl Pts',(-0.497563221603356,9.52000000000001,-1.88052046250904));
#7199=CARTESIAN_POINT('Ctrl Pts',(-0.212605147610961,9.52000000000001,-1.96369393371656));
#7200=CARTESIAN_POINT('Ctrl Pts',(-0.0644024157051228,9.52000000000001,
-1.98948599115583));
#7201=CARTESIAN_POINT('Ctrl Pts',(0.0859174328513603,9.52000000000001,-1.99815344810835));
#7202=CARTESIAN_POINT('Ctrl Pts',(1.6211138875,0.731250000955919,-1.9852919333802E-16));
#7203=CARTESIAN_POINT('Ctrl Pts',(1.6211138875,0.672916667622592,0.935950539335165));
#7204=CARTESIAN_POINT('Ctrl Pts',(0.810556943750001,0.614583334289251,1.40392580900275));
#7205=CARTESIAN_POINT('Ctrl Pts',(3.43862649647115E-16,0.556250000955924,
1.87190107867033));
#7206=CARTESIAN_POINT('Ctrl Pts',(-0.810556943749999,0.497916667622583,
1.40392580900275));
#7207=CARTESIAN_POINT('Ctrl Pts',(-1.6211138875,0.439583334289256,0.935950539335167));
#7208=CARTESIAN_POINT('Ctrl Pts',(-1.6211138875,0.381250000955916,0.));
#7209=CARTESIAN_POINT('Ctrl Pts',(-1.6211138875,0.322916667622589,-0.935950539335166));
#7210=CARTESIAN_POINT('Ctrl Pts',(-0.81055694375,0.264583334289248,-1.40392580900275));
#7211=CARTESIAN_POINT('Ctrl Pts',(-1.14620883215705E-16,0.206250000955921,
-1.87190107867033));
#7212=CARTESIAN_POINT('Ctrl Pts',(0.81055694375,0.147916667622594,-1.40392580900275));
#7213=CARTESIAN_POINT('Ctrl Pts',(1.37954992065153,0.106967962856252,-1.07541756062164));
#7214=CARTESIAN_POINT('Ctrl Pts',(1.55927926836488,0.0611138874999995,-0.443461835441161));
#7215=CARTESIAN_POINT('Origin',(-2.77555756156289E-16,71.6937500009559,
-2.08166817117217E-16));
#7216=CARTESIAN_POINT('Ctrl Pts',(1.6211138875,0.556250000955924,-1.9852919333802E-16));
#7217=CARTESIAN_POINT('Ctrl Pts',(1.6211138875,0.497916667622597,0.935950539335165));
#7218=CARTESIAN_POINT('Ctrl Pts',(0.810556943750001,0.439583334289256,1.40392580900275));
#7219=CARTESIAN_POINT('Ctrl Pts',(3.43862649647115E-16,0.381250000955929,
1.87190107867033));
#7220=CARTESIAN_POINT('Ctrl Pts',(-0.810556943749999,0.322916667622589,
1.40392580900275));
#7221=CARTESIAN_POINT('Ctrl Pts',(-1.6211138875,0.264583334289262,0.935950539335167));
#7222=CARTESIAN_POINT('Ctrl Pts',(-1.6211138875,0.206250000955921,0.));
#7223=CARTESIAN_POINT('Ctrl Pts',(-1.6211138875,0.147916667622594,-0.935950539335166));
#7224=CARTESIAN_POINT('Ctrl Pts',(-0.81055694375,0.0895833342892532,-1.40392580900275));
#7225=CARTESIAN_POINT('Ctrl Pts',(-0.623625223172666,0.0761304233604275,
-1.51185088819815));
#7226=CARTESIAN_POINT('Ctrl Pts',(-0.414966524668622,0.0611138874999821,
-1.56710338511853));
#7227=CARTESIAN_POINT('Ctrl Pts',(-2.00612458230317,71.3839639726704,0.));
#7228=CARTESIAN_POINT('Ctrl Pts',(-2.00612458230317,71.3256306393371,-1.15823656762066));
#7229=CARTESIAN_POINT('Ctrl Pts',(-1.00306229115158,71.2672973060038,-1.73735485143099));
#7230=CARTESIAN_POINT('Ctrl Pts',(-1.41843070519206E-16,71.2089639726704,
-2.31647313524132));
#7231=CARTESIAN_POINT('Ctrl Pts',(1.00306229115158,71.1506306393371,-1.73735485143099));
#7232=CARTESIAN_POINT('Ctrl Pts',(2.00612458230317,71.0922973060038,-1.15823656762066));
#7233=CARTESIAN_POINT('Ctrl Pts',(2.00612458230317,71.0339639726704,-2.45679404840839E-16));
#7234=CARTESIAN_POINT('Ctrl Pts',(2.00612458230317,70.9756306393371,1.15823656762066));
#7235=CARTESIAN_POINT('Ctrl Pts',(1.00306229115158,70.9172973060038,1.73735485143099));
#7236=CARTESIAN_POINT('Ctrl Pts',(4.25529211557617E-16,70.8589639726704,
2.31647313524132));
#7237=CARTESIAN_POINT('Ctrl Pts',(-1.00306229115158,70.8006306393371,1.73735485143099));
#7238=CARTESIAN_POINT('Ctrl Pts',(-2.00612458230316,70.7422973060038,1.15823656762066));
#7239=CARTESIAN_POINT('Ctrl Pts',(-2.00612458230317,70.6839639726704,0.));
#7240=CARTESIAN_POINT('Ctrl Pts',(-2.00612458230317,70.6256306393371,-1.15823656762066));
#7241=CARTESIAN_POINT('Ctrl Pts',(-1.00306229115158,70.5672973060038,-1.73735485143099));
#7242=CARTESIAN_POINT('Ctrl Pts',(-1.41843070519206E-16,70.5089639726704,
-2.31647313524132));
#7243=CARTESIAN_POINT('Ctrl Pts',(1.00306229115158,70.4506306393371,-1.73735485143099));
#7244=CARTESIAN_POINT('Ctrl Pts',(2.00612458230317,70.3922973060038,-1.15823656762066));
#7245=CARTESIAN_POINT('Ctrl Pts',(2.00612458230317,70.3339639726704,-2.45679404840839E-16));
#7246=CARTESIAN_POINT('Ctrl Pts',(2.00612458230317,70.2756306393371,1.15823656762066));
#7247=CARTESIAN_POINT('Ctrl Pts',(1.00306229115158,70.2172973060038,1.73735485143099));
#7248=CARTESIAN_POINT('Ctrl Pts',(4.25529211557617E-16,70.1589639726704,
2.31647313524132));
#7249=CARTESIAN_POINT('Ctrl Pts',(-1.00306229115158,70.1006306393371,1.73735485143099));
#7250=CARTESIAN_POINT('Ctrl Pts',(-2.00612458230316,70.0422973060037,1.15823656762066));
#7251=CARTESIAN_POINT('Ctrl Pts',(-2.00612458230317,69.9839639726704,0.));
#7252=CARTESIAN_POINT('Ctrl Pts',(-2.00612458230317,69.9256306393371,-1.15823656762066));
#7253=CARTESIAN_POINT('Ctrl Pts',(-1.00306229115158,69.8672973060038,-1.73735485143099));
#7254=CARTESIAN_POINT('Ctrl Pts',(-1.41843070519206E-16,69.8089639726704,
-2.31647313524132));
#7255=CARTESIAN_POINT('Ctrl Pts',(1.00306229115158,69.7506306393371,-1.73735485143099));
#7256=CARTESIAN_POINT('Ctrl Pts',(2.00612458230317,69.6922973060038,-1.15823656762066));
#7257=CARTESIAN_POINT('Ctrl Pts',(2.00612458230317,69.6339639726704,-2.45679404840839E-16));
#7258=CARTESIAN_POINT('Ctrl Pts',(2.00612458230317,69.5756306393371,1.15823656762066));
#7259=CARTESIAN_POINT('Ctrl Pts',(1.00306229115158,69.5172973060038,1.73735485143099));
#7260=CARTESIAN_POINT('Ctrl Pts',(4.25529211557617E-16,69.4589639726704,
2.31647313524132));
#7261=CARTESIAN_POINT('Ctrl Pts',(-1.00306229115158,69.4006306393371,1.73735485143099));
#7262=CARTESIAN_POINT('Ctrl Pts',(-2.00612458230316,69.3422973060038,1.15823656762066));
#7263=CARTESIAN_POINT('Ctrl Pts',(-2.00612458230317,69.2839639726704,0.));
#7264=CARTESIAN_POINT('Ctrl Pts',(-2.00612458230317,69.2256306393371,-1.15823656762066));
#7265=CARTESIAN_POINT('Ctrl Pts',(-1.00306229115158,69.1672973060038,-1.73735485143099));
#7266=CARTESIAN_POINT('Ctrl Pts',(-1.41843070519206E-16,69.1089639726704,
-2.31647313524132));
#7267=CARTESIAN_POINT('Ctrl Pts',(1.00306229115158,69.0506306393371,-1.73735485143099));
#7268=CARTESIAN_POINT('Ctrl Pts',(2.00612458230317,68.9922973060038,-1.15823656762066));
#7269=CARTESIAN_POINT('Ctrl Pts',(2.00612458230317,68.9339639726704,-2.45679404840839E-16));
#7270=CARTESIAN_POINT('Ctrl Pts',(2.00612458230317,68.8756306393371,1.15823656762066));
#7271=CARTESIAN_POINT('Ctrl Pts',(1.00306229115158,68.8172973060038,1.73735485143099));
#7272=CARTESIAN_POINT('Ctrl Pts',(4.25529211557617E-16,68.7589639726704,
2.31647313524132));
#7273=CARTESIAN_POINT('Ctrl Pts',(-1.00306229115158,68.7006306393371,1.73735485143099));
#7274=CARTESIAN_POINT('Ctrl Pts',(-2.00612458230316,68.6422973060037,1.15823656762066));
#7275=CARTESIAN_POINT('Ctrl Pts',(-2.00612458230317,68.5839639726704,0.));
#7276=CARTESIAN_POINT('Ctrl Pts',(-2.00612458230317,68.5256306393371,-1.15823656762066));
#7277=CARTESIAN_POINT('Ctrl Pts',(-1.00306229115158,68.4672973060038,-1.73735485143099));
#7278=CARTESIAN_POINT('Ctrl Pts',(-1.41843070519206E-16,68.4089639726704,
-2.31647313524132));
#7279=CARTESIAN_POINT('Ctrl Pts',(1.00306229115158,68.3506306393371,-1.73735485143099));
#7280=CARTESIAN_POINT('Ctrl Pts',(2.00612458230317,68.2922973060038,-1.15823656762066));
#7281=CARTESIAN_POINT('Ctrl Pts',(2.00612458230317,68.2339639726704,-2.45679404840839E-16));
#7282=CARTESIAN_POINT('Ctrl Pts',(2.00612458230317,68.1756306393371,1.15823656762066));
#7283=CARTESIAN_POINT('Ctrl Pts',(1.00306229115158,68.1172973060038,1.73735485143099));
#7284=CARTESIAN_POINT('Ctrl Pts',(4.25529211557617E-16,68.0589639726704,
2.31647313524132));
#7285=CARTESIAN_POINT('Ctrl Pts',(-1.00306229115158,68.0006306393371,1.73735485143099));
#7286=CARTESIAN_POINT('Ctrl Pts',(-2.00612458230316,67.9422973060038,1.15823656762066));
#7287=CARTESIAN_POINT('Ctrl Pts',(-2.00612458230317,67.8839639726704,0.));
#7288=CARTESIAN_POINT('Ctrl Pts',(-2.00612458230317,67.8256306393371,-1.15823656762066));
#7289=CARTESIAN_POINT('Ctrl Pts',(-1.00306229115158,67.7672973060038,-1.73735485143099));
#7290=CARTESIAN_POINT('Ctrl Pts',(-1.41843070519206E-16,67.7089639726704,
-2.31647313524132));
#7291=CARTESIAN_POINT('Ctrl Pts',(1.00306229115158,67.6506306393371,-1.73735485143099));
#7292=CARTESIAN_POINT('Ctrl Pts',(2.00612458230317,67.5922973060038,-1.15823656762066));
#7293=CARTESIAN_POINT('Ctrl Pts',(2.00612458230317,67.5339639726704,-2.45679404840839E-16));
#7294=CARTESIAN_POINT('Ctrl Pts',(2.00612458230317,67.4756306393371,1.15823656762066));
#7295=CARTESIAN_POINT('Ctrl Pts',(1.00306229115158,67.4172973060038,1.73735485143099));
#7296=CARTESIAN_POINT('Ctrl Pts',(4.25529211557617E-16,67.3589639726704,
2.31647313524132));
#7297=CARTESIAN_POINT('Ctrl Pts',(-1.00306229115158,67.3006306393371,1.73735485143099));
#7298=CARTESIAN_POINT('Ctrl Pts',(-2.00612458230316,67.2422973060038,1.15823656762066));
#7299=CARTESIAN_POINT('Ctrl Pts',(-2.00612458230317,67.1839639726704,0.));
#7300=CARTESIAN_POINT('Ctrl Pts',(-2.00612458230317,67.1256306393371,-1.15823656762066));
#7301=CARTESIAN_POINT('Ctrl Pts',(-1.00306229115158,67.0672973060038,-1.73735485143099));
#7302=CARTESIAN_POINT('Ctrl Pts',(-1.41843070519206E-16,67.0089639726704,
-2.31647313524132));
#7303=CARTESIAN_POINT('Ctrl Pts',(1.00306229115158,66.9506306393371,-1.73735485143099));
#7304=CARTESIAN_POINT('Ctrl Pts',(2.00612458230317,66.8922973060038,-1.15823656762066));
#7305=CARTESIAN_POINT('Ctrl Pts',(2.00612458230317,66.8339639726704,-2.45679404840839E-16));
#7306=CARTESIAN_POINT('Ctrl Pts',(2.00612458230317,66.7756306393371,1.15823656762066));
#7307=CARTESIAN_POINT('Ctrl Pts',(1.00306229115158,66.7172973060038,1.73735485143099));
#7308=CARTESIAN_POINT('Ctrl Pts',(4.25529211557617E-16,66.6589639726704,
2.31647313524132));
#7309=CARTESIAN_POINT('Ctrl Pts',(-1.00306229115158,66.6006306393371,1.73735485143099));
#7310=CARTESIAN_POINT('Ctrl Pts',(-2.00612458230316,66.5422973060038,1.15823656762066));
#7311=CARTESIAN_POINT('Ctrl Pts',(-2.00612458230317,66.4839639726704,0.));
#7312=CARTESIAN_POINT('Ctrl Pts',(-2.00612458230317,66.4256306393371,-1.15823656762066));
#7313=CARTESIAN_POINT('Ctrl Pts',(-1.00306229115158,66.3672973060038,-1.73735485143099));
#7314=CARTESIAN_POINT('Ctrl Pts',(-1.41843070519206E-16,66.3089639726704,
-2.31647313524132));
#7315=CARTESIAN_POINT('Ctrl Pts',(1.00306229115158,66.2506306393371,-1.73735485143099));
#7316=CARTESIAN_POINT('Ctrl Pts',(2.00612458230317,66.1922973060038,-1.15823656762066));
#7317=CARTESIAN_POINT('Ctrl Pts',(2.00612458230317,66.1339639726704,-2.45679404840839E-16));
#7318=CARTESIAN_POINT('Ctrl Pts',(2.00612458230317,66.0756306393371,1.15823656762066));
#7319=CARTESIAN_POINT('Ctrl Pts',(1.00306229115158,66.0172973060038,1.73735485143099));
#7320=CARTESIAN_POINT('Ctrl Pts',(4.25529211557617E-16,65.9589639726704,
2.31647313524132));
#7321=CARTESIAN_POINT('Ctrl Pts',(-1.00306229115158,65.9006306393371,1.73735485143099));
#7322=CARTESIAN_POINT('Ctrl Pts',(-2.00612458230316,65.8422973060038,1.15823656762066));
#7323=CARTESIAN_POINT('Ctrl Pts',(-2.00612458230317,65.7839639726704,0.));
#7324=CARTESIAN_POINT('Ctrl Pts',(-2.00612458230317,65.7256306393371,-1.15823656762066));
#7325=CARTESIAN_POINT('Ctrl Pts',(-1.00306229115158,65.6672973060038,-1.73735485143099));
#7326=CARTESIAN_POINT('Ctrl Pts',(-1.41843070519206E-16,65.6089639726704,
-2.31647313524132));
#7327=CARTESIAN_POINT('Ctrl Pts',(1.00306229115158,65.5506306393371,-1.73735485143099));
#7328=CARTESIAN_POINT('Ctrl Pts',(2.00612458230317,65.4922973060037,-1.15823656762066));
#7329=CARTESIAN_POINT('Ctrl Pts',(2.00612458230317,65.4339639726704,-2.45679404840839E-16));
#7330=CARTESIAN_POINT('Ctrl Pts',(2.00612458230317,65.3756306393371,1.15823656762066));
#7331=CARTESIAN_POINT('Ctrl Pts',(1.00306229115158,65.3172973060038,1.73735485143099));
#7332=CARTESIAN_POINT('Ctrl Pts',(4.25529211557617E-16,65.2589639726704,
2.31647313524132));
#7333=CARTESIAN_POINT('Ctrl Pts',(-1.00306229115158,65.2006306393371,1.73735485143099));
#7334=CARTESIAN_POINT('Ctrl Pts',(-2.00612458230316,65.1422973060038,1.15823656762066));
#7335=CARTESIAN_POINT('Ctrl Pts',(-2.00612458230317,65.0839639726704,0.));
#7336=CARTESIAN_POINT('Ctrl Pts',(-2.00612458230317,65.0256306393371,-1.15823656762066));
#7337=CARTESIAN_POINT('Ctrl Pts',(-1.00306229115158,64.9672973060038,-1.73735485143099));
#7338=CARTESIAN_POINT('Ctrl Pts',(-1.41843070519206E-16,64.9089639726704,
-2.31647313524132));
#7339=CARTESIAN_POINT('Ctrl Pts',(1.00306229115158,64.8506306393371,-1.73735485143099));
#7340=CARTESIAN_POINT('Ctrl Pts',(2.00612458230317,64.7922973060038,-1.15823656762066));
#7341=CARTESIAN_POINT('Ctrl Pts',(2.00612458230317,64.7339639726704,-2.45679404840839E-16));
#7342=CARTESIAN_POINT('Ctrl Pts',(2.00612458230317,64.6756306393371,1.15823656762066));
#7343=CARTESIAN_POINT('Ctrl Pts',(1.00306229115158,64.6172973060038,1.73735485143099));
#7344=CARTESIAN_POINT('Ctrl Pts',(4.25529211557617E-16,64.5589639726704,
2.31647313524132));
#7345=CARTESIAN_POINT('Ctrl Pts',(-1.00306229115158,64.5006306393371,1.73735485143099));
#7346=CARTESIAN_POINT('Ctrl Pts',(-2.00612458230316,64.4422973060038,1.15823656762066));
#7347=CARTESIAN_POINT('Ctrl Pts',(-2.00612458230317,64.3839639726704,0.));
#7348=CARTESIAN_POINT('Ctrl Pts',(-2.00612458230317,64.3256306393371,-1.15823656762066));
#7349=CARTESIAN_POINT('Ctrl Pts',(-1.00306229115158,64.2672973060038,-1.73735485143099));
#7350=CARTESIAN_POINT('Ctrl Pts',(-1.41843070519206E-16,64.2089639726704,
-2.31647313524132));
#7351=CARTESIAN_POINT('Ctrl Pts',(1.00306229115158,64.1506306393371,-1.73735485143099));
#7352=CARTESIAN_POINT('Ctrl Pts',(2.00612458230317,64.0922973060038,-1.15823656762066));
#7353=CARTESIAN_POINT('Ctrl Pts',(2.00612458230317,64.0339639726704,-2.45679404840839E-16));
#7354=CARTESIAN_POINT('Ctrl Pts',(2.00612458230317,63.9756306393371,1.15823656762066));
#7355=CARTESIAN_POINT('Ctrl Pts',(1.00306229115158,63.9172973060038,1.73735485143099));
#7356=CARTESIAN_POINT('Ctrl Pts',(4.25529211557617E-16,63.8589639726704,
2.31647313524132));
#7357=CARTESIAN_POINT('Ctrl Pts',(-1.00306229115158,63.8006306393371,1.73735485143099));
#7358=CARTESIAN_POINT('Ctrl Pts',(-2.00612458230316,63.7422973060038,1.15823656762066));
#7359=CARTESIAN_POINT('Ctrl Pts',(-2.00612458230317,63.6839639726704,0.));
#7360=CARTESIAN_POINT('Ctrl Pts',(-2.00612458230317,63.6256306393371,-1.15823656762066));
#7361=CARTESIAN_POINT('Ctrl Pts',(-1.00306229115158,63.5672973060038,-1.73735485143099));
#7362=CARTESIAN_POINT('Ctrl Pts',(-1.41843070519206E-16,63.5089639726704,
-2.31647313524132));
#7363=CARTESIAN_POINT('Ctrl Pts',(1.00306229115158,63.4506306393371,-1.73735485143099));
#7364=CARTESIAN_POINT('Ctrl Pts',(2.00612458230317,63.3922973060038,-1.15823656762066));
#7365=CARTESIAN_POINT('Ctrl Pts',(2.00612458230317,63.3339639726704,-2.45679404840839E-16));
#7366=CARTESIAN_POINT('Ctrl Pts',(2.00612458230317,63.2756306393371,1.15823656762066));
#7367=CARTESIAN_POINT('Ctrl Pts',(1.00306229115158,63.2172973060038,1.73735485143099));
#7368=CARTESIAN_POINT('Ctrl Pts',(4.25529211557617E-16,63.1589639726704,
2.31647313524132));
#7369=CARTESIAN_POINT('Ctrl Pts',(-1.00306229115158,63.1006306393371,1.73735485143099));
#7370=CARTESIAN_POINT('Ctrl Pts',(-2.00612458230316,63.0422973060038,1.15823656762066));
#7371=CARTESIAN_POINT('Ctrl Pts',(-2.00612458230317,62.9839639726704,0.));
#7372=CARTESIAN_POINT('Ctrl Pts',(-2.00612458230317,62.9256306393371,-1.15823656762066));
#7373=CARTESIAN_POINT('Ctrl Pts',(-1.00306229115158,62.8672973060038,-1.73735485143099));
#7374=CARTESIAN_POINT('Ctrl Pts',(-1.41843070519206E-16,62.8089639726704,
-2.31647313524132));
#7375=CARTESIAN_POINT('Ctrl Pts',(1.00306229115158,62.7506306393371,-1.73735485143099));
#7376=CARTESIAN_POINT('Ctrl Pts',(2.00612458230317,62.6922973060038,-1.15823656762066));
#7377=CARTESIAN_POINT('Ctrl Pts',(2.00612458230317,62.6339639726704,-2.45679404840839E-16));
#7378=CARTESIAN_POINT('Ctrl Pts',(2.00612458230317,62.5756306393371,1.15823656762066));
#7379=CARTESIAN_POINT('Ctrl Pts',(1.00306229115158,62.5172973060038,1.73735485143099));
#7380=CARTESIAN_POINT('Ctrl Pts',(4.25529211557617E-16,62.4589639726704,
2.31647313524132));
#7381=CARTESIAN_POINT('Ctrl Pts',(-1.00306229115158,62.4006306393371,1.73735485143099));
#7382=CARTESIAN_POINT('Ctrl Pts',(-2.00612458230316,62.3422973060038,1.15823656762066));
#7383=CARTESIAN_POINT('Ctrl Pts',(-2.00612458230317,62.2839639726704,0.));
#7384=CARTESIAN_POINT('Ctrl Pts',(-2.00612458230317,62.2256306393371,-1.15823656762066));
#7385=CARTESIAN_POINT('Ctrl Pts',(-1.00306229115158,62.1672973060038,-1.73735485143099));
#7386=CARTESIAN_POINT('Ctrl Pts',(-1.41843070519206E-16,62.1089639726704,
-2.31647313524132));
#7387=CARTESIAN_POINT('Ctrl Pts',(1.00306229115158,62.0506306393371,-1.73735485143099));
#7388=CARTESIAN_POINT('Ctrl Pts',(2.00612458230317,61.9922973060038,-1.15823656762066));
#7389=CARTESIAN_POINT('Ctrl Pts',(2.00612458230317,61.9339639726704,-2.45679404840839E-16));
#7390=CARTESIAN_POINT('Ctrl Pts',(2.00612458230317,61.8756306393371,1.15823656762066));
#7391=CARTESIAN_POINT('Ctrl Pts',(1.00306229115158,61.8172973060038,1.73735485143099));
#7392=CARTESIAN_POINT('Ctrl Pts',(4.25529211557617E-16,61.7589639726704,
2.31647313524132));
#7393=CARTESIAN_POINT('Ctrl Pts',(-1.00306229115158,61.7006306393371,1.73735485143099));
#7394=CARTESIAN_POINT('Ctrl Pts',(-2.00612458230316,61.6422973060038,1.15823656762066));
#7395=CARTESIAN_POINT('Ctrl Pts',(-2.00612458230317,61.5839639726704,0.));
#7396=CARTESIAN_POINT('Ctrl Pts',(-2.00612458230317,61.5256306393371,-1.15823656762066));
#7397=CARTESIAN_POINT('Ctrl Pts',(-1.00306229115158,61.4672973060038,-1.73735485143099));
#7398=CARTESIAN_POINT('Ctrl Pts',(-1.41843070519206E-16,61.4089639726704,
-2.31647313524132));
#7399=CARTESIAN_POINT('Ctrl Pts',(1.00306229115158,61.3506306393371,-1.73735485143099));
#7400=CARTESIAN_POINT('Ctrl Pts',(2.00612458230317,61.2922973060038,-1.15823656762066));
#7401=CARTESIAN_POINT('Ctrl Pts',(2.00612458230317,61.2339639726704,-2.45679404840839E-16));
#7402=CARTESIAN_POINT('Ctrl Pts',(2.00612458230317,61.1756306393371,1.15823656762066));
#7403=CARTESIAN_POINT('Ctrl Pts',(1.00306229115158,61.1172973060038,1.73735485143099));
#7404=CARTESIAN_POINT('Ctrl Pts',(4.25529211557617E-16,61.0589639726704,
2.31647313524132));
#7405=CARTESIAN_POINT('Ctrl Pts',(-1.00306229115158,61.0006306393371,1.73735485143099));
#7406=CARTESIAN_POINT('Ctrl Pts',(-2.00612458230316,60.9422973060038,1.15823656762066));
#7407=CARTESIAN_POINT('Ctrl Pts',(-2.00612458230317,60.8839639726704,0.));
#7408=CARTESIAN_POINT('Ctrl Pts',(-2.00612458230317,60.8256306393371,-1.15823656762066));
#7409=CARTESIAN_POINT('Ctrl Pts',(-1.00306229115158,60.7672973060038,-1.73735485143099));
#7410=CARTESIAN_POINT('Ctrl Pts',(-1.41843070519206E-16,60.7089639726704,
-2.31647313524132));
#7411=CARTESIAN_POINT('Ctrl Pts',(1.00306229115158,60.6506306393371,-1.73735485143099));
#7412=CARTESIAN_POINT('Ctrl Pts',(2.00612458230317,60.5922973060038,-1.15823656762066));
#7413=CARTESIAN_POINT('Ctrl Pts',(2.00612458230317,60.5339639726704,-2.45679404840839E-16));
#7414=CARTESIAN_POINT('Ctrl Pts',(2.00612458230317,60.4756306393371,1.15823656762066));
#7415=CARTESIAN_POINT('Ctrl Pts',(1.00306229115158,60.4172973060038,1.73735485143099));
#7416=CARTESIAN_POINT('Ctrl Pts',(4.25529211557617E-16,60.3589639726704,
2.31647313524132));
#7417=CARTESIAN_POINT('Ctrl Pts',(-1.00306229115158,60.3006306393371,1.73735485143099));
#7418=CARTESIAN_POINT('Ctrl Pts',(-2.00612458230316,60.2422973060038,1.15823656762066));
#7419=CARTESIAN_POINT('Ctrl Pts',(-2.00612458230317,60.1839639726704,0.));
#7420=CARTESIAN_POINT('Ctrl Pts',(-2.00612458230317,60.1256306393371,-1.15823656762066));
#7421=CARTESIAN_POINT('Ctrl Pts',(-1.00306229115158,60.0672973060038,-1.73735485143099));
#7422=CARTESIAN_POINT('Ctrl Pts',(-1.41843070519206E-16,60.0089639726704,
-2.31647313524132));
#7423=CARTESIAN_POINT('Ctrl Pts',(1.00306229115158,59.9506306393371,-1.73735485143099));
#7424=CARTESIAN_POINT('Ctrl Pts',(2.00612458230317,59.8922973060038,-1.15823656762066));
#7425=CARTESIAN_POINT('Ctrl Pts',(2.00612458230317,59.8339639726704,-2.45679404840839E-16));
#7426=CARTESIAN_POINT('Ctrl Pts',(2.00612458230317,59.7756306393371,1.15823656762066));
#7427=CARTESIAN_POINT('Ctrl Pts',(1.00306229115158,59.7172973060038,1.73735485143099));
#7428=CARTESIAN_POINT('Ctrl Pts',(4.25529211557617E-16,59.6589639726704,
2.31647313524132));
#7429=CARTESIAN_POINT('Ctrl Pts',(-1.00306229115158,59.6006306393371,1.73735485143099));
#7430=CARTESIAN_POINT('Ctrl Pts',(-2.00612458230316,59.5422973060038,1.15823656762066));
#7431=CARTESIAN_POINT('Ctrl Pts',(-2.00612458230317,59.4839639726704,0.));
#7432=CARTESIAN_POINT('Ctrl Pts',(-2.00612458230317,59.4256306393371,-1.15823656762066));
#7433=CARTESIAN_POINT('Ctrl Pts',(-1.00306229115158,59.3672973060038,-1.73735485143099));
#7434=CARTESIAN_POINT('Ctrl Pts',(-1.41843070519206E-16,59.3089639726704,
-2.31647313524132));
#7435=CARTESIAN_POINT('Ctrl Pts',(1.00306229115158,59.2506306393371,-1.73735485143099));
#7436=CARTESIAN_POINT('Ctrl Pts',(2.00612458230317,59.1922973060038,-1.15823656762066));
#7437=CARTESIAN_POINT('Ctrl Pts',(2.00612458230317,59.1339639726704,-2.45679404840839E-16));
#7438=CARTESIAN_POINT('Ctrl Pts',(2.00612458230317,59.0756306393371,1.15823656762066));
#7439=CARTESIAN_POINT('Ctrl Pts',(1.00306229115158,59.0172973060038,1.73735485143099));
#7440=CARTESIAN_POINT('Ctrl Pts',(4.25529211557617E-16,58.9589639726704,
2.31647313524132));
#7441=CARTESIAN_POINT('Ctrl Pts',(-1.00306229115158,58.9006306393371,1.73735485143099));
#7442=CARTESIAN_POINT('Ctrl Pts',(-2.00612458230316,58.8422973060038,1.15823656762066));
#7443=CARTESIAN_POINT('Ctrl Pts',(-2.00612458230317,58.7839639726704,0.));
#7444=CARTESIAN_POINT('Ctrl Pts',(-2.00612458230317,58.7256306393371,-1.15823656762066));
#7445=CARTESIAN_POINT('Ctrl Pts',(-1.00306229115158,58.6672973060038,-1.73735485143099));
#7446=CARTESIAN_POINT('Ctrl Pts',(-1.41843070519206E-16,58.6089639726704,
-2.31647313524132));
#7447=CARTESIAN_POINT('Ctrl Pts',(1.00306229115158,58.5506306393371,-1.73735485143099));
#7448=CARTESIAN_POINT('Ctrl Pts',(2.00612458230317,58.4922973060038,-1.15823656762066));
#7449=CARTESIAN_POINT('Ctrl Pts',(2.00612458230317,58.4339639726704,-2.45679404840839E-16));
#7450=CARTESIAN_POINT('Ctrl Pts',(2.00612458230317,58.3756306393371,1.15823656762066));
#7451=CARTESIAN_POINT('Ctrl Pts',(1.00306229115158,58.3172973060038,1.73735485143099));
#7452=CARTESIAN_POINT('Ctrl Pts',(4.25529211557617E-16,58.2589639726704,
2.31647313524132));
#7453=CARTESIAN_POINT('Ctrl Pts',(-1.00306229115158,58.2006306393371,1.73735485143099));
#7454=CARTESIAN_POINT('Ctrl Pts',(-2.00612458230316,58.1422973060038,1.15823656762066));
#7455=CARTESIAN_POINT('Ctrl Pts',(-2.00612458230317,58.0839639726704,0.));
#7456=CARTESIAN_POINT('Ctrl Pts',(-2.00612458230317,58.0256306393371,-1.15823656762066));
#7457=CARTESIAN_POINT('Ctrl Pts',(-1.00306229115158,57.9672973060038,-1.73735485143099));
#7458=CARTESIAN_POINT('Ctrl Pts',(-1.41843070519206E-16,57.9089639726704,
-2.31647313524132));
#7459=CARTESIAN_POINT('Ctrl Pts',(1.00306229115158,57.8506306393371,-1.73735485143099));
#7460=CARTESIAN_POINT('Ctrl Pts',(2.00612458230317,57.7922973060038,-1.15823656762066));
#7461=CARTESIAN_POINT('Ctrl Pts',(2.00612458230317,57.7339639726704,-2.45679404840839E-16));
#7462=CARTESIAN_POINT('Ctrl Pts',(2.00612458230317,57.6756306393371,1.15823656762066));
#7463=CARTESIAN_POINT('Ctrl Pts',(1.00306229115158,57.6172973060038,1.73735485143099));
#7464=CARTESIAN_POINT('Ctrl Pts',(4.25529211557617E-16,57.5589639726704,
2.31647313524132));
#7465=CARTESIAN_POINT('Ctrl Pts',(-1.00306229115158,57.5006306393371,1.73735485143099));
#7466=CARTESIAN_POINT('Ctrl Pts',(-2.00612458230316,57.4422973060038,1.15823656762066));
#7467=CARTESIAN_POINT('Ctrl Pts',(-2.00612458230317,57.3839639726704,0.));
#7468=CARTESIAN_POINT('Ctrl Pts',(-2.00612458230317,57.3256306393371,-1.15823656762066));
#7469=CARTESIAN_POINT('Ctrl Pts',(-1.00306229115158,57.2672973060038,-1.73735485143099));
#7470=CARTESIAN_POINT('Ctrl Pts',(-1.41843070519206E-16,57.2089639726704,
-2.31647313524132));
#7471=CARTESIAN_POINT('Ctrl Pts',(1.00306229115158,57.1506306393371,-1.73735485143099));
#7472=CARTESIAN_POINT('Ctrl Pts',(2.00612458230317,57.0922973060038,-1.15823656762066));
#7473=CARTESIAN_POINT('Ctrl Pts',(2.00612458230317,57.0339639726704,-2.45679404840839E-16));
#7474=CARTESIAN_POINT('Ctrl Pts',(2.00612458230317,56.9756306393371,1.15823656762066));
#7475=CARTESIAN_POINT('Ctrl Pts',(1.00306229115158,56.9172973060038,1.73735485143099));
#7476=CARTESIAN_POINT('Ctrl Pts',(4.25529211557617E-16,56.8589639726704,
2.31647313524132));
#7477=CARTESIAN_POINT('Ctrl Pts',(-1.00306229115158,56.8006306393371,1.73735485143099));
#7478=CARTESIAN_POINT('Ctrl Pts',(-2.00612458230316,56.7422973060038,1.15823656762066));
#7479=CARTESIAN_POINT('Ctrl Pts',(-2.00612458230317,56.6839639726704,0.));
#7480=CARTESIAN_POINT('Ctrl Pts',(-2.00612458230317,56.6256306393371,-1.15823656762066));
#7481=CARTESIAN_POINT('Ctrl Pts',(-1.00306229115158,56.5672973060038,-1.73735485143099));
#7482=CARTESIAN_POINT('Ctrl Pts',(-1.41843070519206E-16,56.5089639726704,
-2.31647313524132));
#7483=CARTESIAN_POINT('Ctrl Pts',(1.00306229115158,56.4506306393371,-1.73735485143099));
#7484=CARTESIAN_POINT('Ctrl Pts',(2.00612458230317,56.3922973060038,-1.15823656762066));
#7485=CARTESIAN_POINT('Ctrl Pts',(2.00612458230317,56.3339639726704,-2.45679404840839E-16));
#7486=CARTESIAN_POINT('Ctrl Pts',(2.00612458230317,56.2756306393371,1.15823656762066));
#7487=CARTESIAN_POINT('Ctrl Pts',(1.00306229115158,56.2172973060038,1.73735485143099));
#7488=CARTESIAN_POINT('Ctrl Pts',(4.25529211557617E-16,56.1589639726704,
2.31647313524132));
#7489=CARTESIAN_POINT('Ctrl Pts',(-1.00306229115158,56.1006306393371,1.73735485143099));
#7490=CARTESIAN_POINT('Ctrl Pts',(-2.00612458230316,56.0422973060038,1.15823656762066));
#7491=CARTESIAN_POINT('Ctrl Pts',(-2.00612458230317,55.9839639726704,0.));
#7492=CARTESIAN_POINT('Ctrl Pts',(-2.00612458230317,55.9256306393371,-1.15823656762066));
#7493=CARTESIAN_POINT('Ctrl Pts',(-1.00306229115158,55.8672973060038,-1.73735485143099));
#7494=CARTESIAN_POINT('Ctrl Pts',(-1.41843070519206E-16,55.8089639726704,
-2.31647313524132));
#7495=CARTESIAN_POINT('Ctrl Pts',(1.00306229115158,55.7506306393371,-1.73735485143099));
#7496=CARTESIAN_POINT('Ctrl Pts',(2.00612458230317,55.6922973060038,-1.15823656762066));
#7497=CARTESIAN_POINT('Ctrl Pts',(2.00612458230317,55.6339639726704,-2.45679404840839E-16));
#7498=CARTESIAN_POINT('Ctrl Pts',(2.00612458230317,55.5756306393371,1.15823656762066));
#7499=CARTESIAN_POINT('Ctrl Pts',(1.00306229115158,55.5172973060038,1.73735485143099));
#7500=CARTESIAN_POINT('Ctrl Pts',(4.25529211557617E-16,55.4589639726704,
2.31647313524132));
#7501=CARTESIAN_POINT('Ctrl Pts',(-1.00306229115158,55.4006306393371,1.73735485143099));
#7502=CARTESIAN_POINT('Ctrl Pts',(-2.00612458230316,55.3422973060038,1.15823656762066));
#7503=CARTESIAN_POINT('Ctrl Pts',(-2.00612458230317,55.2839639726704,0.));
#7504=CARTESIAN_POINT('Ctrl Pts',(-2.00612458230317,55.2256306393371,-1.15823656762066));
#7505=CARTESIAN_POINT('Ctrl Pts',(-1.00306229115158,55.1672973060038,-1.73735485143099));
#7506=CARTESIAN_POINT('Ctrl Pts',(-1.41843070519206E-16,55.1089639726704,
-2.31647313524132));
#7507=CARTESIAN_POINT('Ctrl Pts',(1.00306229115158,55.0506306393371,-1.73735485143099));
#7508=CARTESIAN_POINT('Ctrl Pts',(2.00612458230317,54.9922973060038,-1.15823656762066));
#7509=CARTESIAN_POINT('Ctrl Pts',(2.00612458230317,54.9339639726704,-2.45679404840839E-16));
#7510=CARTESIAN_POINT('Ctrl Pts',(2.00612458230317,54.8756306393371,1.15823656762066));
#7511=CARTESIAN_POINT('Ctrl Pts',(1.00306229115158,54.8172973060038,1.73735485143099));
#7512=CARTESIAN_POINT('Ctrl Pts',(4.25529211557617E-16,54.7589639726704,
2.31647313524132));
#7513=CARTESIAN_POINT('Ctrl Pts',(-1.00306229115158,54.7006306393371,1.73735485143099));
#7514=CARTESIAN_POINT('Ctrl Pts',(-2.00612458230316,54.6422973060038,1.15823656762066));
#7515=CARTESIAN_POINT('Ctrl Pts',(-2.00612458230317,54.5839639726704,0.));
#7516=CARTESIAN_POINT('Ctrl Pts',(-2.00612458230317,54.5256306393371,-1.15823656762066));
#7517=CARTESIAN_POINT('Ctrl Pts',(-1.00306229115158,54.4672973060038,-1.73735485143099));
#7518=CARTESIAN_POINT('Ctrl Pts',(-1.41843070519206E-16,54.4089639726704,
-2.31647313524132));
#7519=CARTESIAN_POINT('Ctrl Pts',(1.00306229115158,54.3506306393371,-1.73735485143099));
#7520=CARTESIAN_POINT('Ctrl Pts',(2.00612458230317,54.2922973060038,-1.15823656762066));
#7521=CARTESIAN_POINT('Ctrl Pts',(2.00612458230317,54.2339639726704,-2.45679404840839E-16));
#7522=CARTESIAN_POINT('Ctrl Pts',(2.00612458230317,54.1756306393371,1.15823656762066));
#7523=CARTESIAN_POINT('Ctrl Pts',(1.00306229115158,54.1172973060038,1.73735485143099));
#7524=CARTESIAN_POINT('Ctrl Pts',(4.25529211557617E-16,54.0589639726704,
2.31647313524132));
#7525=CARTESIAN_POINT('Ctrl Pts',(-1.00306229115158,54.0006306393371,1.73735485143099));
#7526=CARTESIAN_POINT('Ctrl Pts',(-2.00612458230316,53.9422973060038,1.15823656762066));
#7527=CARTESIAN_POINT('Ctrl Pts',(-2.00612458230317,53.8839639726704,0.));
#7528=CARTESIAN_POINT('Ctrl Pts',(-2.00612458230317,53.8256306393371,-1.15823656762066));
#7529=CARTESIAN_POINT('Ctrl Pts',(-1.00306229115158,53.7672973060038,-1.73735485143099));
#7530=CARTESIAN_POINT('Ctrl Pts',(-1.41843070519206E-16,53.7089639726704,
-2.31647313524132));
#7531=CARTESIAN_POINT('Ctrl Pts',(1.00306229115158,53.6506306393371,-1.73735485143099));
#7532=CARTESIAN_POINT('Ctrl Pts',(2.00612458230317,53.5922973060038,-1.15823656762066));
#7533=CARTESIAN_POINT('Ctrl Pts',(2.00612458230317,53.5339639726704,-2.45679404840839E-16));
#7534=CARTESIAN_POINT('Ctrl Pts',(2.00612458230317,53.4756306393371,1.15823656762066));
#7535=CARTESIAN_POINT('Ctrl Pts',(1.00306229115158,53.4172973060038,1.73735485143099));
#7536=CARTESIAN_POINT('Ctrl Pts',(4.25529211557617E-16,53.3589639726704,
2.31647313524132));
#7537=CARTESIAN_POINT('Ctrl Pts',(-1.00306229115158,53.3006306393371,1.73735485143099));
#7538=CARTESIAN_POINT('Ctrl Pts',(-2.00612458230316,53.2422973060038,1.15823656762066));
#7539=CARTESIAN_POINT('Ctrl Pts',(-2.00612458230317,53.1839639726704,0.));
#7540=CARTESIAN_POINT('Ctrl Pts',(-2.00612458230317,53.1256306393371,-1.15823656762066));
#7541=CARTESIAN_POINT('Ctrl Pts',(-1.00306229115158,53.0672973060038,-1.73735485143099));
#7542=CARTESIAN_POINT('Ctrl Pts',(-1.41843070519206E-16,53.0089639726704,
-2.31647313524132));
#7543=CARTESIAN_POINT('Ctrl Pts',(1.00306229115158,52.9506306393371,-1.73735485143099));
#7544=CARTESIAN_POINT('Ctrl Pts',(2.00612458230317,52.8922973060038,-1.15823656762066));
#7545=CARTESIAN_POINT('Ctrl Pts',(2.00612458230317,52.8339639726704,-2.45679404840839E-16));
#7546=CARTESIAN_POINT('Ctrl Pts',(2.00612458230317,52.7756306393371,1.15823656762066));
#7547=CARTESIAN_POINT('Ctrl Pts',(1.00306229115158,52.7172973060038,1.73735485143099));
#7548=CARTESIAN_POINT('Ctrl Pts',(4.25529211557617E-16,52.6589639726704,
2.31647313524132));
#7549=CARTESIAN_POINT('Ctrl Pts',(-1.00306229115158,52.6006306393371,1.73735485143099));
#7550=CARTESIAN_POINT('Ctrl Pts',(-2.00612458230316,52.5422973060038,1.15823656762066));
#7551=CARTESIAN_POINT('Ctrl Pts',(-2.00612458230317,52.4839639726704,0.));
#7552=CARTESIAN_POINT('Ctrl Pts',(-2.00612458230317,52.4256306393371,-1.15823656762066));
#7553=CARTESIAN_POINT('Ctrl Pts',(-1.00306229115158,52.3672973060038,-1.73735485143099));
#7554=CARTESIAN_POINT('Ctrl Pts',(-1.41843070519206E-16,52.3089639726704,
-2.31647313524132));
#7555=CARTESIAN_POINT('Ctrl Pts',(1.00306229115158,52.2506306393371,-1.73735485143099));
#7556=CARTESIAN_POINT('Ctrl Pts',(2.00612458230317,52.1922973060038,-1.15823656762066));
#7557=CARTESIAN_POINT('Ctrl Pts',(2.00612458230317,52.1339639726704,-2.45679404840839E-16));
#7558=CARTESIAN_POINT('Ctrl Pts',(2.00612458230317,52.0756306393371,1.15823656762066));
#7559=CARTESIAN_POINT('Ctrl Pts',(1.00306229115158,52.0172973060038,1.73735485143099));
#7560=CARTESIAN_POINT('Ctrl Pts',(4.25529211557617E-16,51.9589639726704,
2.31647313524132));
#7561=CARTESIAN_POINT('Ctrl Pts',(-1.00306229115158,51.9006306393371,1.73735485143099));
#7562=CARTESIAN_POINT('Ctrl Pts',(-2.00612458230316,51.8422973060038,1.15823656762066));
#7563=CARTESIAN_POINT('Ctrl Pts',(-2.00612458230317,51.7839639726704,0.));
#7564=CARTESIAN_POINT('Ctrl Pts',(-2.00612458230317,51.7256306393371,-1.15823656762066));
#7565=CARTESIAN_POINT('Ctrl Pts',(-1.00306229115158,51.6672973060038,-1.73735485143099));
#7566=CARTESIAN_POINT('Ctrl Pts',(-1.41843070519206E-16,51.6089639726704,
-2.31647313524132));
#7567=CARTESIAN_POINT('Ctrl Pts',(1.00306229115158,51.5506306393371,-1.73735485143099));
#7568=CARTESIAN_POINT('Ctrl Pts',(2.00612458230317,51.4922973060038,-1.15823656762066));
#7569=CARTESIAN_POINT('Ctrl Pts',(2.00612458230317,51.4339639726704,-2.45679404840839E-16));
#7570=CARTESIAN_POINT('Ctrl Pts',(2.00612458230317,51.3756306393371,1.15823656762066));
#7571=CARTESIAN_POINT('Ctrl Pts',(1.00306229115158,51.3172973060038,1.73735485143099));
#7572=CARTESIAN_POINT('Ctrl Pts',(4.25529211557617E-16,51.2589639726704,
2.31647313524132));
#7573=CARTESIAN_POINT('Ctrl Pts',(-1.00306229115158,51.2006306393371,1.73735485143099));
#7574=CARTESIAN_POINT('Ctrl Pts',(-2.00612458230316,51.1422973060038,1.15823656762066));
#7575=CARTESIAN_POINT('Ctrl Pts',(-2.00612458230317,51.0839639726704,0.));
#7576=CARTESIAN_POINT('Ctrl Pts',(-2.00612458230317,51.0256306393371,-1.15823656762066));
#7577=CARTESIAN_POINT('Ctrl Pts',(-1.00306229115158,50.9672973060038,-1.73735485143099));
#7578=CARTESIAN_POINT('Ctrl Pts',(-1.41843070519206E-16,50.9089639726704,
-2.31647313524132));
#7579=CARTESIAN_POINT('Ctrl Pts',(1.00306229115158,50.8506306393371,-1.73735485143099));
#7580=CARTESIAN_POINT('Ctrl Pts',(2.00612458230317,50.7922973060038,-1.15823656762066));
#7581=CARTESIAN_POINT('Ctrl Pts',(2.00612458230317,50.7339639726704,-2.45679404840839E-16));
#7582=CARTESIAN_POINT('Ctrl Pts',(2.00612458230317,50.6756306393371,1.15823656762066));
#7583=CARTESIAN_POINT('Ctrl Pts',(1.00306229115158,50.6172973060038,1.73735485143099));
#7584=CARTESIAN_POINT('Ctrl Pts',(4.25529211557617E-16,50.5589639726704,
2.31647313524132));
#7585=CARTESIAN_POINT('Ctrl Pts',(-1.00306229115158,50.5006306393371,1.73735485143099));
#7586=CARTESIAN_POINT('Ctrl Pts',(-2.00612458230316,50.4422973060038,1.15823656762066));
#7587=CARTESIAN_POINT('Ctrl Pts',(-2.00612458230317,50.3839639726704,0.));
#7588=CARTESIAN_POINT('Ctrl Pts',(-2.00612458230317,50.3256306393371,-1.15823656762066));
#7589=CARTESIAN_POINT('Ctrl Pts',(-1.00306229115158,50.2672973060038,-1.73735485143099));
#7590=CARTESIAN_POINT('Ctrl Pts',(-1.41843070519206E-16,50.2089639726704,
-2.31647313524132));
#7591=CARTESIAN_POINT('Ctrl Pts',(1.00306229115158,50.1506306393371,-1.73735485143099));
#7592=CARTESIAN_POINT('Ctrl Pts',(2.00612458230317,50.0922973060038,-1.15823656762066));
#7593=CARTESIAN_POINT('Ctrl Pts',(2.00612458230317,50.0339639726704,-2.45679404840839E-16));
#7594=CARTESIAN_POINT('Ctrl Pts',(2.00612458230317,49.9756306393371,1.15823656762066));
#7595=CARTESIAN_POINT('Ctrl Pts',(1.00306229115158,49.9172973060038,1.73735485143099));
#7596=CARTESIAN_POINT('Ctrl Pts',(4.25529211557617E-16,49.8589639726704,
2.31647313524132));
#7597=CARTESIAN_POINT('Ctrl Pts',(-1.00306229115158,49.8006306393371,1.73735485143099));
#7598=CARTESIAN_POINT('Ctrl Pts',(-2.00612458230316,49.7422973060038,1.15823656762066));
#7599=CARTESIAN_POINT('Ctrl Pts',(-2.00612458230317,49.6839639726704,0.));
#7600=CARTESIAN_POINT('Ctrl Pts',(-2.00612458230317,49.6256306393371,-1.15823656762066));
#7601=CARTESIAN_POINT('Ctrl Pts',(-1.00306229115158,49.5672973060038,-1.73735485143099));
#7602=CARTESIAN_POINT('Ctrl Pts',(-1.41843070519206E-16,49.5089639726704,
-2.31647313524132));
#7603=CARTESIAN_POINT('Ctrl Pts',(1.00306229115158,49.4506306393371,-1.73735485143099));
#7604=CARTESIAN_POINT('Ctrl Pts',(2.00612458230317,49.3922973060038,-1.15823656762066));
#7605=CARTESIAN_POINT('Ctrl Pts',(2.00612458230317,49.3339639726704,-2.45679404840839E-16));
#7606=CARTESIAN_POINT('Ctrl Pts',(2.00612458230317,49.2756306393371,1.15823656762066));
#7607=CARTESIAN_POINT('Ctrl Pts',(1.00306229115158,49.2172973060038,1.73735485143099));
#7608=CARTESIAN_POINT('Ctrl Pts',(4.25529211557617E-16,49.1589639726704,
2.31647313524132));
#7609=CARTESIAN_POINT('Ctrl Pts',(-1.00306229115158,49.1006306393371,1.73735485143099));
#7610=CARTESIAN_POINT('Ctrl Pts',(-2.00612458230316,49.0422973060038,1.15823656762066));
#7611=CARTESIAN_POINT('Ctrl Pts',(-2.00612458230317,48.9839639726704,0.));
#7612=CARTESIAN_POINT('Ctrl Pts',(-2.00612458230317,48.9256306393371,-1.15823656762066));
#7613=CARTESIAN_POINT('Ctrl Pts',(-1.00306229115158,48.8672973060038,-1.73735485143099));
#7614=CARTESIAN_POINT('Ctrl Pts',(-1.41843070519206E-16,48.8089639726704,
-2.31647313524132));
#7615=CARTESIAN_POINT('Ctrl Pts',(1.00306229115158,48.7506306393371,-1.73735485143099));
#7616=CARTESIAN_POINT('Ctrl Pts',(2.00612458230317,48.6922973060038,-1.15823656762066));
#7617=CARTESIAN_POINT('Ctrl Pts',(2.00612458230317,48.6339639726704,-2.45679404840839E-16));
#7618=CARTESIAN_POINT('Ctrl Pts',(2.00612458230317,48.5756306393371,1.15823656762066));
#7619=CARTESIAN_POINT('Ctrl Pts',(1.00306229115158,48.5172973060038,1.73735485143099));
#7620=CARTESIAN_POINT('Ctrl Pts',(4.25529211557617E-16,48.4589639726704,
2.31647313524132));
#7621=CARTESIAN_POINT('Ctrl Pts',(-1.00306229115158,48.4006306393371,1.73735485143099));
#7622=CARTESIAN_POINT('Ctrl Pts',(-2.00612458230316,48.3422973060038,1.15823656762066));
#7623=CARTESIAN_POINT('Ctrl Pts',(-2.00612458230317,48.2839639726704,0.));
#7624=CARTESIAN_POINT('Ctrl Pts',(-2.00612458230317,48.2256306393371,-1.15823656762066));
#7625=CARTESIAN_POINT('Ctrl Pts',(-1.00306229115158,48.1672973060038,-1.73735485143099));
#7626=CARTESIAN_POINT('Ctrl Pts',(-1.41843070519206E-16,48.1089639726704,
-2.31647313524132));
#7627=CARTESIAN_POINT('Ctrl Pts',(1.00306229115158,48.0506306393371,-1.73735485143099));
#7628=CARTESIAN_POINT('Ctrl Pts',(2.00612458230317,47.9922973060037,-1.15823656762066));
#7629=CARTESIAN_POINT('Ctrl Pts',(2.00612458230317,47.9339639726704,-2.45679404840839E-16));
#7630=CARTESIAN_POINT('Ctrl Pts',(2.00612458230317,47.8756306393371,1.15823656762066));
#7631=CARTESIAN_POINT('Ctrl Pts',(1.00306229115158,47.8172973060038,1.73735485143099));
#7632=CARTESIAN_POINT('Ctrl Pts',(4.25529211557617E-16,47.7589639726704,
2.31647313524132));
#7633=CARTESIAN_POINT('Ctrl Pts',(-1.00306229115158,47.7006306393371,1.73735485143099));
#7634=CARTESIAN_POINT('Ctrl Pts',(-2.00612458230316,47.6422973060038,1.15823656762066));
#7635=CARTESIAN_POINT('Ctrl Pts',(-2.00612458230317,47.5839639726704,0.));
#7636=CARTESIAN_POINT('Ctrl Pts',(-2.00612458230317,47.5256306393371,-1.15823656762066));
#7637=CARTESIAN_POINT('Ctrl Pts',(-1.00306229115158,47.4672973060038,-1.73735485143099));
#7638=CARTESIAN_POINT('Ctrl Pts',(-1.41843070519206E-16,47.4089639726704,
-2.31647313524132));
#7639=CARTESIAN_POINT('Ctrl Pts',(1.00306229115158,47.3506306393371,-1.73735485143099));
#7640=CARTESIAN_POINT('Ctrl Pts',(2.00612458230317,47.2922973060038,-1.15823656762066));
#7641=CARTESIAN_POINT('Ctrl Pts',(2.00612458230317,47.2339639726704,-2.45679404840839E-16));
#7642=CARTESIAN_POINT('Ctrl Pts',(2.00612458230317,47.1756306393371,1.15823656762066));
#7643=CARTESIAN_POINT('Ctrl Pts',(1.00306229115158,47.1172973060038,1.73735485143099));
#7644=CARTESIAN_POINT('Ctrl Pts',(4.25529211557617E-16,47.0589639726704,
2.31647313524132));
#7645=CARTESIAN_POINT('Ctrl Pts',(-1.00306229115158,47.0006306393371,1.73735485143099));
#7646=CARTESIAN_POINT('Ctrl Pts',(-2.00612458230316,46.9422973060038,1.15823656762066));
#7647=CARTESIAN_POINT('Ctrl Pts',(-2.00612458230317,46.8839639726704,0.));
#7648=CARTESIAN_POINT('Ctrl Pts',(-2.00612458230317,46.8256306393371,-1.15823656762066));
#7649=CARTESIAN_POINT('Ctrl Pts',(-1.00306229115158,46.7672973060038,-1.73735485143099));
#7650=CARTESIAN_POINT('Ctrl Pts',(-1.41843070519206E-16,46.7089639726704,
-2.31647313524132));
#7651=CARTESIAN_POINT('Ctrl Pts',(1.00306229115158,46.6506306393371,-1.73735485143099));
#7652=CARTESIAN_POINT('Ctrl Pts',(2.00612458230317,46.5922973060038,-1.15823656762066));
#7653=CARTESIAN_POINT('Ctrl Pts',(2.00612458230317,46.5339639726704,-2.45679404840839E-16));
#7654=CARTESIAN_POINT('Ctrl Pts',(2.00612458230317,46.4756306393371,1.15823656762066));
#7655=CARTESIAN_POINT('Ctrl Pts',(1.00306229115158,46.4172973060038,1.73735485143099));
#7656=CARTESIAN_POINT('Ctrl Pts',(4.25529211557617E-16,46.3589639726704,
2.31647313524132));
#7657=CARTESIAN_POINT('Ctrl Pts',(-1.00306229115158,46.3006306393371,1.73735485143099));
#7658=CARTESIAN_POINT('Ctrl Pts',(-2.00612458230316,46.2422973060038,1.15823656762066));
#7659=CARTESIAN_POINT('Ctrl Pts',(-2.00612458230317,46.1839639726704,0.));
#7660=CARTESIAN_POINT('Ctrl Pts',(-2.00612458230317,46.1256306393371,-1.15823656762066));
#7661=CARTESIAN_POINT('Ctrl Pts',(-1.00306229115158,46.0672973060038,-1.73735485143099));
#7662=CARTESIAN_POINT('Ctrl Pts',(-1.41843070519206E-16,46.0089639726704,
-2.31647313524132));
#7663=CARTESIAN_POINT('Ctrl Pts',(1.00306229115158,45.9506306393371,-1.73735485143099));
#7664=CARTESIAN_POINT('Ctrl Pts',(2.00612458230317,45.8922973060038,-1.15823656762066));
#7665=CARTESIAN_POINT('Ctrl Pts',(2.00612458230317,45.8339639726704,-2.45679404840839E-16));
#7666=CARTESIAN_POINT('Ctrl Pts',(2.00612458230317,45.7756306393371,1.15823656762066));
#7667=CARTESIAN_POINT('Ctrl Pts',(1.00306229115158,45.7172973060038,1.73735485143099));
#7668=CARTESIAN_POINT('Ctrl Pts',(4.25529211557617E-16,45.6589639726704,
2.31647313524132));
#7669=CARTESIAN_POINT('Ctrl Pts',(-1.00306229115158,45.6006306393371,1.73735485143099));
#7670=CARTESIAN_POINT('Ctrl Pts',(-2.00612458230316,45.5422973060038,1.15823656762066));
#7671=CARTESIAN_POINT('Ctrl Pts',(-2.00612458230317,45.4839639726704,0.));
#7672=CARTESIAN_POINT('Ctrl Pts',(-2.00612458230317,45.4256306393371,-1.15823656762066));
#7673=CARTESIAN_POINT('Ctrl Pts',(-1.00306229115158,45.3672973060038,-1.73735485143099));
#7674=CARTESIAN_POINT('Ctrl Pts',(-1.41843070519206E-16,45.3089639726704,
-2.31647313524132));
#7675=CARTESIAN_POINT('Ctrl Pts',(1.00306229115158,45.2506306393371,-1.73735485143099));
#7676=CARTESIAN_POINT('Ctrl Pts',(2.00612458230317,45.1922973060038,-1.15823656762066));
#7677=CARTESIAN_POINT('Ctrl Pts',(2.00612458230317,45.1339639726704,-2.45679404840839E-16));
#7678=CARTESIAN_POINT('Ctrl Pts',(2.00612458230317,45.0756306393371,1.15823656762066));
#7679=CARTESIAN_POINT('Ctrl Pts',(1.00306229115158,45.0172973060038,1.73735485143099));
#7680=CARTESIAN_POINT('Ctrl Pts',(4.25529211557617E-16,44.9589639726704,
2.31647313524132));
#7681=CARTESIAN_POINT('Ctrl Pts',(-1.00306229115158,44.9006306393371,1.73735485143099));
#7682=CARTESIAN_POINT('Ctrl Pts',(-2.00612458230316,44.8422973060038,1.15823656762066));
#7683=CARTESIAN_POINT('Ctrl Pts',(-2.00612458230317,44.7839639726704,0.));
#7684=CARTESIAN_POINT('Ctrl Pts',(-2.00612458230317,44.7256306393371,-1.15823656762066));
#7685=CARTESIAN_POINT('Ctrl Pts',(-1.00306229115158,44.6672973060038,-1.73735485143099));
#7686=CARTESIAN_POINT('Ctrl Pts',(-1.41843070519206E-16,44.6089639726704,
-2.31647313524132));
#7687=CARTESIAN_POINT('Ctrl Pts',(1.00306229115158,44.5506306393371,-1.73735485143099));
#7688=CARTESIAN_POINT('Ctrl Pts',(2.00612458230317,44.4922973060038,-1.15823656762066));
#7689=CARTESIAN_POINT('Ctrl Pts',(2.00612458230317,44.4339639726704,-2.45679404840839E-16));
#7690=CARTESIAN_POINT('Ctrl Pts',(2.00612458230317,44.3756306393371,1.15823656762066));
#7691=CARTESIAN_POINT('Ctrl Pts',(1.00306229115158,44.3172973060038,1.73735485143099));
#7692=CARTESIAN_POINT('Ctrl Pts',(4.25529211557617E-16,44.2589639726704,
2.31647313524132));
#7693=CARTESIAN_POINT('Ctrl Pts',(-1.00306229115158,44.2006306393371,1.73735485143099));
#7694=CARTESIAN_POINT('Ctrl Pts',(-2.00612458230316,44.1422973060038,1.15823656762066));
#7695=CARTESIAN_POINT('Ctrl Pts',(-2.00612458230317,44.0839639726704,0.));
#7696=CARTESIAN_POINT('Ctrl Pts',(-2.00612458230317,44.0256306393371,-1.15823656762066));
#7697=CARTESIAN_POINT('Ctrl Pts',(-1.00306229115158,43.9672973060038,-1.73735485143099));
#7698=CARTESIAN_POINT('Ctrl Pts',(-1.41843070519206E-16,43.9089639726704,
-2.31647313524132));
#7699=CARTESIAN_POINT('Ctrl Pts',(1.00306229115158,43.8506306393371,-1.73735485143099));
#7700=CARTESIAN_POINT('Ctrl Pts',(2.00612458230317,43.7922973060038,-1.15823656762066));
#7701=CARTESIAN_POINT('Ctrl Pts',(2.00612458230317,43.7339639726704,-2.45679404840839E-16));
#7702=CARTESIAN_POINT('Ctrl Pts',(2.00612458230317,43.6756306393371,1.15823656762066));
#7703=CARTESIAN_POINT('Ctrl Pts',(1.00306229115158,43.6172973060038,1.73735485143099));
#7704=CARTESIAN_POINT('Ctrl Pts',(4.25529211557617E-16,43.5589639726704,
2.31647313524132));
#7705=CARTESIAN_POINT('Ctrl Pts',(-1.00306229115158,43.5006306393371,1.73735485143099));
#7706=CARTESIAN_POINT('Ctrl Pts',(-2.00612458230316,43.4422973060038,1.15823656762066));
#7707=CARTESIAN_POINT('Ctrl Pts',(-2.00612458230317,43.3839639726704,0.));
#7708=CARTESIAN_POINT('Ctrl Pts',(-2.00612458230317,43.3256306393371,-1.15823656762066));
#7709=CARTESIAN_POINT('Ctrl Pts',(-1.00306229115158,43.2672973060038,-1.73735485143099));
#7710=CARTESIAN_POINT('Ctrl Pts',(-1.41843070519206E-16,43.2089639726704,
-2.31647313524132));
#7711=CARTESIAN_POINT('Ctrl Pts',(1.00306229115158,43.1506306393371,-1.73735485143099));
#7712=CARTESIAN_POINT('Ctrl Pts',(2.00612458230317,43.0922973060038,-1.15823656762066));
#7713=CARTESIAN_POINT('Ctrl Pts',(2.00612458230317,43.0339639726704,-2.45679404840839E-16));
#7714=CARTESIAN_POINT('Ctrl Pts',(2.00612458230317,42.9756306393371,1.15823656762066));
#7715=CARTESIAN_POINT('Ctrl Pts',(1.00306229115158,42.9172973060038,1.73735485143099));
#7716=CARTESIAN_POINT('Ctrl Pts',(4.25529211557617E-16,42.8589639726704,
2.31647313524132));
#7717=CARTESIAN_POINT('Ctrl Pts',(-1.00306229115158,42.8006306393371,1.73735485143099));
#7718=CARTESIAN_POINT('Ctrl Pts',(-2.00612458230316,42.7422973060038,1.15823656762066));
#7719=CARTESIAN_POINT('Ctrl Pts',(-2.00612458230317,42.6839639726704,0.));
#7720=CARTESIAN_POINT('Ctrl Pts',(-2.00612458230317,42.6256306393371,-1.15823656762066));
#7721=CARTESIAN_POINT('Ctrl Pts',(-1.00306229115158,42.5672973060038,-1.73735485143099));
#7722=CARTESIAN_POINT('Ctrl Pts',(-1.41843070519206E-16,42.5089639726704,
-2.31647313524132));
#7723=CARTESIAN_POINT('Ctrl Pts',(1.00306229115158,42.4506306393371,-1.73735485143099));
#7724=CARTESIAN_POINT('Ctrl Pts',(2.00612458230317,42.3922973060038,-1.15823656762066));
#7725=CARTESIAN_POINT('Ctrl Pts',(2.00612458230317,42.3339639726704,-2.45679404840839E-16));
#7726=CARTESIAN_POINT('Ctrl Pts',(2.00612458230317,42.2756306393371,1.15823656762066));
#7727=CARTESIAN_POINT('Ctrl Pts',(1.00306229115158,42.2172973060038,1.73735485143099));
#7728=CARTESIAN_POINT('Ctrl Pts',(4.25529211557617E-16,42.1589639726704,
2.31647313524132));
#7729=CARTESIAN_POINT('Ctrl Pts',(-1.00306229115158,42.1006306393371,1.73735485143099));
#7730=CARTESIAN_POINT('Ctrl Pts',(-2.00612458230316,42.0422973060038,1.15823656762066));
#7731=CARTESIAN_POINT('Ctrl Pts',(-2.00612458230317,41.9839639726704,0.));
#7732=CARTESIAN_POINT('Ctrl Pts',(-2.00612458230317,41.9256306393371,-1.15823656762066));
#7733=CARTESIAN_POINT('Ctrl Pts',(-1.00306229115158,41.8672973060038,-1.73735485143099));
#7734=CARTESIAN_POINT('Ctrl Pts',(-1.41843070519206E-16,41.8089639726704,
-2.31647313524132));
#7735=CARTESIAN_POINT('Ctrl Pts',(1.00306229115158,41.7506306393371,-1.73735485143099));
#7736=CARTESIAN_POINT('Ctrl Pts',(2.00612458230317,41.6922973060038,-1.15823656762066));
#7737=CARTESIAN_POINT('Ctrl Pts',(2.00612458230317,41.6339639726704,-2.45679404840839E-16));
#7738=CARTESIAN_POINT('Ctrl Pts',(2.00612458230317,41.5756306393371,1.15823656762066));
#7739=CARTESIAN_POINT('Ctrl Pts',(1.00306229115158,41.5172973060038,1.73735485143099));
#7740=CARTESIAN_POINT('Ctrl Pts',(4.25529211557617E-16,41.4589639726704,
2.31647313524132));
#7741=CARTESIAN_POINT('Ctrl Pts',(-1.00306229115158,41.4006306393371,1.73735485143099));
#7742=CARTESIAN_POINT('Ctrl Pts',(-2.00612458230316,41.3422973060038,1.15823656762066));
#7743=CARTESIAN_POINT('Ctrl Pts',(-2.00612458230317,41.2839639726704,0.));
#7744=CARTESIAN_POINT('Ctrl Pts',(-2.00612458230317,41.2256306393371,-1.15823656762066));
#7745=CARTESIAN_POINT('Ctrl Pts',(-1.00306229115158,41.1672973060038,-1.73735485143099));
#7746=CARTESIAN_POINT('Ctrl Pts',(-1.41843070519206E-16,41.1089639726704,
-2.31647313524132));
#7747=CARTESIAN_POINT('Ctrl Pts',(1.00306229115158,41.0506306393371,-1.73735485143099));
#7748=CARTESIAN_POINT('Ctrl Pts',(2.00612458230317,40.9922973060038,-1.15823656762066));
#7749=CARTESIAN_POINT('Ctrl Pts',(2.00612458230317,40.9339639726704,-2.45679404840839E-16));
#7750=CARTESIAN_POINT('Ctrl Pts',(2.00612458230317,40.8756306393371,1.15823656762066));
#7751=CARTESIAN_POINT('Ctrl Pts',(1.00306229115158,40.8172973060038,1.73735485143099));
#7752=CARTESIAN_POINT('Ctrl Pts',(4.25529211557617E-16,40.7589639726704,
2.31647313524132));
#7753=CARTESIAN_POINT('Ctrl Pts',(-1.00306229115158,40.7006306393371,1.73735485143099));
#7754=CARTESIAN_POINT('Ctrl Pts',(-2.00612458230316,40.6422973060038,1.15823656762066));
#7755=CARTESIAN_POINT('Ctrl Pts',(-2.00612458230317,40.5839639726704,0.));
#7756=CARTESIAN_POINT('Ctrl Pts',(-2.00612458230317,40.5256306393371,-1.15823656762066));
#7757=CARTESIAN_POINT('Ctrl Pts',(-1.00306229115158,40.4672973060038,-1.73735485143099));
#7758=CARTESIAN_POINT('Ctrl Pts',(-1.41843070519206E-16,40.4089639726704,
-2.31647313524132));
#7759=CARTESIAN_POINT('Ctrl Pts',(1.00306229115158,40.3506306393371,-1.73735485143099));
#7760=CARTESIAN_POINT('Ctrl Pts',(2.00612458230317,40.2922973060038,-1.15823656762066));
#7761=CARTESIAN_POINT('Ctrl Pts',(2.00612458230317,40.2339639726704,-2.45679404840839E-16));
#7762=CARTESIAN_POINT('Ctrl Pts',(2.00612458230317,40.1756306393371,1.15823656762066));
#7763=CARTESIAN_POINT('Ctrl Pts',(1.00306229115158,40.1172973060038,1.73735485143099));
#7764=CARTESIAN_POINT('Ctrl Pts',(4.25529211557617E-16,40.0589639726704,
2.31647313524132));
#7765=CARTESIAN_POINT('Ctrl Pts',(-1.00306229115158,40.0006306393371,1.73735485143099));
#7766=CARTESIAN_POINT('Ctrl Pts',(-2.00612458230316,39.9422973060038,1.15823656762066));
#7767=CARTESIAN_POINT('Ctrl Pts',(-2.00612458230317,39.8839639726704,0.));
#7768=CARTESIAN_POINT('Ctrl Pts',(-2.00612458230317,39.8256306393371,-1.15823656762066));
#7769=CARTESIAN_POINT('Ctrl Pts',(-1.00306229115158,39.7672973060038,-1.73735485143099));
#7770=CARTESIAN_POINT('Ctrl Pts',(-1.41843070519206E-16,39.7089639726704,
-2.31647313524132));
#7771=CARTESIAN_POINT('Ctrl Pts',(1.00306229115158,39.6506306393371,-1.73735485143099));
#7772=CARTESIAN_POINT('Ctrl Pts',(2.00612458230317,39.5922973060038,-1.15823656762066));
#7773=CARTESIAN_POINT('Ctrl Pts',(2.00612458230317,39.5339639726704,-2.45679404840839E-16));
#7774=CARTESIAN_POINT('Ctrl Pts',(2.00612458230317,39.4756306393371,1.15823656762066));
#7775=CARTESIAN_POINT('Ctrl Pts',(1.00306229115158,39.4172973060038,1.73735485143099));
#7776=CARTESIAN_POINT('Ctrl Pts',(4.25529211557617E-16,39.3589639726704,
2.31647313524132));
#7777=CARTESIAN_POINT('Ctrl Pts',(-1.00306229115158,39.3006306393371,1.73735485143099));
#7778=CARTESIAN_POINT('Ctrl Pts',(-2.00612458230316,39.2422973060038,1.15823656762066));
#7779=CARTESIAN_POINT('Ctrl Pts',(-2.00612458230317,39.1839639726704,0.));
#7780=CARTESIAN_POINT('Ctrl Pts',(-2.00612458230317,39.1256306393371,-1.15823656762066));
#7781=CARTESIAN_POINT('Ctrl Pts',(-1.00306229115158,39.0672973060038,-1.73735485143099));
#7782=CARTESIAN_POINT('Ctrl Pts',(-1.41843070519206E-16,39.0089639726704,
-2.31647313524132));
#7783=CARTESIAN_POINT('Ctrl Pts',(1.00306229115158,38.9506306393371,-1.73735485143099));
#7784=CARTESIAN_POINT('Ctrl Pts',(2.00612458230317,38.8922973060038,-1.15823656762066));
#7785=CARTESIAN_POINT('Ctrl Pts',(2.00612458230317,38.8339639726704,-2.45679404840839E-16));
#7786=CARTESIAN_POINT('Ctrl Pts',(2.00612458230317,38.7756306393371,1.15823656762066));
#7787=CARTESIAN_POINT('Ctrl Pts',(1.00306229115158,38.7172973060038,1.73735485143099));
#7788=CARTESIAN_POINT('Ctrl Pts',(4.25529211557617E-16,38.6589639726704,
2.31647313524132));
#7789=CARTESIAN_POINT('Ctrl Pts',(-1.00306229115158,38.6006306393371,1.73735485143099));
#7790=CARTESIAN_POINT('Ctrl Pts',(-2.00612458230316,38.5422973060038,1.15823656762066));
#7791=CARTESIAN_POINT('Ctrl Pts',(-2.00612458230317,38.4839639726704,0.));
#7792=CARTESIAN_POINT('Ctrl Pts',(-2.00612458230317,38.4256306393371,-1.15823656762066));
#7793=CARTESIAN_POINT('Ctrl Pts',(-1.00306229115158,38.3672973060038,-1.73735485143099));
#7794=CARTESIAN_POINT('Ctrl Pts',(-1.41843070519206E-16,38.3089639726704,
-2.31647313524132));
#7795=CARTESIAN_POINT('Ctrl Pts',(1.00306229115158,38.2506306393371,-1.73735485143099));
#7796=CARTESIAN_POINT('Ctrl Pts',(2.00612458230317,38.1922973060038,-1.15823656762066));
#7797=CARTESIAN_POINT('Ctrl Pts',(2.00612458230317,38.1339639726704,-2.45679404840839E-16));
#7798=CARTESIAN_POINT('Ctrl Pts',(2.00612458230317,38.0756306393371,1.15823656762066));
#7799=CARTESIAN_POINT('Ctrl Pts',(1.00306229115158,38.0172973060038,1.73735485143099));
#7800=CARTESIAN_POINT('Ctrl Pts',(4.25529211557617E-16,37.9589639726704,
2.31647313524132));
#7801=CARTESIAN_POINT('Ctrl Pts',(-1.00306229115158,37.9006306393371,1.73735485143099));
#7802=CARTESIAN_POINT('Ctrl Pts',(-2.00612458230316,37.8422973060038,1.15823656762066));
#7803=CARTESIAN_POINT('Ctrl Pts',(-2.00612458230317,37.7839639726704,0.));
#7804=CARTESIAN_POINT('Ctrl Pts',(-2.00612458230317,37.7256306393371,-1.15823656762066));
#7805=CARTESIAN_POINT('Ctrl Pts',(-1.00306229115158,37.6672973060038,-1.73735485143099));
#7806=CARTESIAN_POINT('Ctrl Pts',(-1.41843070519206E-16,37.6089639726704,
-2.31647313524132));
#7807=CARTESIAN_POINT('Ctrl Pts',(1.00306229115158,37.5506306393371,-1.73735485143099));
#7808=CARTESIAN_POINT('Ctrl Pts',(2.00612458230317,37.4922973060038,-1.15823656762066));
#7809=CARTESIAN_POINT('Ctrl Pts',(2.00612458230317,37.4339639726704,-2.45679404840839E-16));
#7810=CARTESIAN_POINT('Ctrl Pts',(2.00612458230317,37.3756306393371,1.15823656762066));
#7811=CARTESIAN_POINT('Ctrl Pts',(1.00306229115158,37.3172973060038,1.73735485143099));
#7812=CARTESIAN_POINT('Ctrl Pts',(4.25529211557617E-16,37.2589639726704,
2.31647313524132));
#7813=CARTESIAN_POINT('Ctrl Pts',(-1.00306229115158,37.2006306393371,1.73735485143099));
#7814=CARTESIAN_POINT('Ctrl Pts',(-2.00612458230316,37.1422973060038,1.15823656762066));
#7815=CARTESIAN_POINT('Ctrl Pts',(-2.00612458230317,37.0839639726704,0.));
#7816=CARTESIAN_POINT('Ctrl Pts',(-2.00612458230317,37.0256306393371,-1.15823656762066));
#7817=CARTESIAN_POINT('Ctrl Pts',(-1.00306229115158,36.9672973060038,-1.73735485143099));
#7818=CARTESIAN_POINT('Ctrl Pts',(-1.41843070519206E-16,36.9089639726704,
-2.31647313524132));
#7819=CARTESIAN_POINT('Ctrl Pts',(1.00306229115158,36.8506306393371,-1.73735485143099));
#7820=CARTESIAN_POINT('Ctrl Pts',(2.00612458230317,36.7922973060038,-1.15823656762066));
#7821=CARTESIAN_POINT('Ctrl Pts',(2.00612458230317,36.7339639726704,-2.45679404840839E-16));
#7822=CARTESIAN_POINT('Ctrl Pts',(2.00612458230317,36.6756306393371,1.15823656762066));
#7823=CARTESIAN_POINT('Ctrl Pts',(1.00306229115158,36.6172973060038,1.73735485143099));
#7824=CARTESIAN_POINT('Ctrl Pts',(4.25529211557617E-16,36.5589639726704,
2.31647313524132));
#7825=CARTESIAN_POINT('Ctrl Pts',(-1.00306229115158,36.5006306393371,1.73735485143099));
#7826=CARTESIAN_POINT('Ctrl Pts',(-2.00612458230316,36.4422973060038,1.15823656762066));
#7827=CARTESIAN_POINT('Ctrl Pts',(-2.00612458230317,36.3839639726704,0.));
#7828=CARTESIAN_POINT('Ctrl Pts',(-2.00612458230317,36.3256306393371,-1.15823656762066));
#7829=CARTESIAN_POINT('Ctrl Pts',(-1.00306229115158,36.2672973060038,-1.73735485143099));
#7830=CARTESIAN_POINT('Ctrl Pts',(-1.41843070519206E-16,36.2089639726704,
-2.31647313524132));
#7831=CARTESIAN_POINT('Ctrl Pts',(1.00306229115158,36.1506306393371,-1.73735485143099));
#7832=CARTESIAN_POINT('Ctrl Pts',(2.00612458230317,36.0922973060038,-1.15823656762066));
#7833=CARTESIAN_POINT('Ctrl Pts',(2.00612458230317,36.0339639726704,-2.45679404840839E-16));
#7834=CARTESIAN_POINT('Ctrl Pts',(2.00612458230317,35.9756306393371,1.15823656762066));
#7835=CARTESIAN_POINT('Ctrl Pts',(1.00306229115158,35.9172973060038,1.73735485143099));
#7836=CARTESIAN_POINT('Ctrl Pts',(4.25529211557617E-16,35.8589639726704,
2.31647313524132));
#7837=CARTESIAN_POINT('Ctrl Pts',(-1.00306229115158,35.8006306393371,1.73735485143099));
#7838=CARTESIAN_POINT('Ctrl Pts',(-2.00612458230316,35.7422973060038,1.15823656762066));
#7839=CARTESIAN_POINT('Ctrl Pts',(-2.00612458230317,35.6839639726704,0.));
#7840=CARTESIAN_POINT('Ctrl Pts',(-2.00612458230317,35.6256306393371,-1.15823656762066));
#7841=CARTESIAN_POINT('Ctrl Pts',(-1.00306229115158,35.5672973060038,-1.73735485143099));
#7842=CARTESIAN_POINT('Ctrl Pts',(-1.41843070519206E-16,35.5089639726704,
-2.31647313524132));
#7843=CARTESIAN_POINT('Ctrl Pts',(1.00306229115158,35.4506306393371,-1.73735485143099));
#7844=CARTESIAN_POINT('Ctrl Pts',(2.00612458230317,35.3922973060038,-1.15823656762066));
#7845=CARTESIAN_POINT('Ctrl Pts',(2.00612458230317,35.3339639726704,-2.45679404840839E-16));
#7846=CARTESIAN_POINT('Ctrl Pts',(2.00612458230317,35.2756306393371,1.15823656762066));
#7847=CARTESIAN_POINT('Ctrl Pts',(1.00306229115158,35.2172973060038,1.73735485143099));
#7848=CARTESIAN_POINT('Ctrl Pts',(4.25529211557617E-16,35.1589639726704,
2.31647313524132));
#7849=CARTESIAN_POINT('Ctrl Pts',(-1.00306229115158,35.1006306393371,1.73735485143099));
#7850=CARTESIAN_POINT('Ctrl Pts',(-2.00612458230316,35.0422973060038,1.15823656762066));
#7851=CARTESIAN_POINT('Ctrl Pts',(-2.00612458230317,34.9839639726704,0.));
#7852=CARTESIAN_POINT('Ctrl Pts',(-2.00612458230317,34.9256306393371,-1.15823656762066));
#7853=CARTESIAN_POINT('Ctrl Pts',(-1.00306229115158,34.8672973060038,-1.73735485143099));
#7854=CARTESIAN_POINT('Ctrl Pts',(-1.41843070519206E-16,34.8089639726704,
-2.31647313524132));
#7855=CARTESIAN_POINT('Ctrl Pts',(1.00306229115158,34.7506306393371,-1.73735485143099));
#7856=CARTESIAN_POINT('Ctrl Pts',(2.00612458230317,34.6922973060038,-1.15823656762066));
#7857=CARTESIAN_POINT('Ctrl Pts',(2.00612458230317,34.6339639726704,-2.45679404840839E-16));
#7858=CARTESIAN_POINT('Ctrl Pts',(2.00612458230317,34.5756306393371,1.15823656762066));
#7859=CARTESIAN_POINT('Ctrl Pts',(1.00306229115158,34.5172973060038,1.73735485143099));
#7860=CARTESIAN_POINT('Ctrl Pts',(4.25529211557617E-16,34.4589639726704,
2.31647313524132));
#7861=CARTESIAN_POINT('Ctrl Pts',(-1.00306229115158,34.4006306393371,1.73735485143099));
#7862=CARTESIAN_POINT('Ctrl Pts',(-2.00612458230316,34.3422973060038,1.15823656762066));
#7863=CARTESIAN_POINT('Ctrl Pts',(-2.00612458230317,34.2839639726704,0.));
#7864=CARTESIAN_POINT('Ctrl Pts',(-2.00612458230317,34.2256306393371,-1.15823656762066));
#7865=CARTESIAN_POINT('Ctrl Pts',(-1.00306229115158,34.1672973060038,-1.73735485143099));
#7866=CARTESIAN_POINT('Ctrl Pts',(-1.41843070519206E-16,34.1089639726704,
-2.31647313524132));
#7867=CARTESIAN_POINT('Ctrl Pts',(1.00306229115158,34.0506306393371,-1.73735485143099));
#7868=CARTESIAN_POINT('Ctrl Pts',(2.00612458230317,33.9922973060038,-1.15823656762066));
#7869=CARTESIAN_POINT('Ctrl Pts',(2.00612458230317,33.9339639726704,-2.45679404840839E-16));
#7870=CARTESIAN_POINT('Ctrl Pts',(2.00612458230317,33.8756306393371,1.15823656762066));
#7871=CARTESIAN_POINT('Ctrl Pts',(1.00306229115158,33.8172973060038,1.73735485143099));
#7872=CARTESIAN_POINT('Ctrl Pts',(4.25529211557617E-16,33.7589639726704,
2.31647313524132));
#7873=CARTESIAN_POINT('Ctrl Pts',(-1.00306229115158,33.7006306393371,1.73735485143099));
#7874=CARTESIAN_POINT('Ctrl Pts',(-2.00612458230316,33.6422973060038,1.15823656762066));
#7875=CARTESIAN_POINT('Ctrl Pts',(-2.00612458230317,33.5839639726704,0.));
#7876=CARTESIAN_POINT('Ctrl Pts',(-2.00612458230317,33.5256306393371,-1.15823656762066));
#7877=CARTESIAN_POINT('Ctrl Pts',(-1.00306229115158,33.4672973060038,-1.73735485143099));
#7878=CARTESIAN_POINT('Ctrl Pts',(-1.41843070519206E-16,33.4089639726704,
-2.31647313524132));
#7879=CARTESIAN_POINT('Ctrl Pts',(1.00306229115158,33.3506306393371,-1.73735485143099));
#7880=CARTESIAN_POINT('Ctrl Pts',(2.00612458230317,33.2922973060038,-1.15823656762066));
#7881=CARTESIAN_POINT('Ctrl Pts',(2.00612458230317,33.2339639726704,-2.45679404840839E-16));
#7882=CARTESIAN_POINT('Ctrl Pts',(2.00612458230317,33.1756306393371,1.15823656762066));
#7883=CARTESIAN_POINT('Ctrl Pts',(1.00306229115158,33.1172973060038,1.73735485143099));
#7884=CARTESIAN_POINT('Ctrl Pts',(4.25529211557617E-16,33.0589639726704,
2.31647313524132));
#7885=CARTESIAN_POINT('Ctrl Pts',(-1.00306229115158,33.0006306393371,1.73735485143099));
#7886=CARTESIAN_POINT('Ctrl Pts',(-2.00612458230316,32.9422973060038,1.15823656762066));
#7887=CARTESIAN_POINT('Ctrl Pts',(-2.00612458230317,32.8839639726704,0.));
#7888=CARTESIAN_POINT('Ctrl Pts',(-2.00612458230317,32.8256306393371,-1.15823656762066));
#7889=CARTESIAN_POINT('Ctrl Pts',(-1.00306229115158,32.7672973060038,-1.73735485143099));
#7890=CARTESIAN_POINT('Ctrl Pts',(-1.41843070519206E-16,32.7089639726704,
-2.31647313524132));
#7891=CARTESIAN_POINT('Ctrl Pts',(1.00306229115158,32.6506306393371,-1.73735485143099));
#7892=CARTESIAN_POINT('Ctrl Pts',(2.00612458230317,32.5922973060038,-1.15823656762066));
#7893=CARTESIAN_POINT('Ctrl Pts',(2.00612458230317,32.5339639726704,-2.45679404840839E-16));
#7894=CARTESIAN_POINT('Ctrl Pts',(2.00612458230317,32.4756306393371,1.15823656762066));
#7895=CARTESIAN_POINT('Ctrl Pts',(1.00306229115158,32.4172973060038,1.73735485143099));
#7896=CARTESIAN_POINT('Ctrl Pts',(4.25529211557617E-16,32.3589639726704,
2.31647313524132));
#7897=CARTESIAN_POINT('Ctrl Pts',(-1.00306229115158,32.3006306393371,1.73735485143099));
#7898=CARTESIAN_POINT('Ctrl Pts',(-2.00612458230316,32.2422973060038,1.15823656762066));
#7899=CARTESIAN_POINT('Ctrl Pts',(-2.00612458230317,32.1839639726704,0.));
#7900=CARTESIAN_POINT('Ctrl Pts',(-2.00612458230317,32.1256306393371,-1.15823656762066));
#7901=CARTESIAN_POINT('Ctrl Pts',(-1.00306229115158,32.0672973060038,-1.73735485143099));
#7902=CARTESIAN_POINT('Ctrl Pts',(-1.41843070519206E-16,32.0089639726704,
-2.31647313524132));
#7903=CARTESIAN_POINT('Ctrl Pts',(1.00306229115158,31.9506306393371,-1.73735485143099));
#7904=CARTESIAN_POINT('Ctrl Pts',(2.00612458230317,31.8922973060038,-1.15823656762066));
#7905=CARTESIAN_POINT('Ctrl Pts',(2.00612458230317,31.8339639726704,-2.45679404840839E-16));
#7906=CARTESIAN_POINT('Ctrl Pts',(2.00612458230317,31.7756306393371,1.15823656762066));
#7907=CARTESIAN_POINT('Ctrl Pts',(1.00306229115158,31.7172973060038,1.73735485143099));
#7908=CARTESIAN_POINT('Ctrl Pts',(4.25529211557617E-16,31.6589639726704,
2.31647313524132));
#7909=CARTESIAN_POINT('Ctrl Pts',(-1.00306229115158,31.6006306393371,1.73735485143099));
#7910=CARTESIAN_POINT('Ctrl Pts',(-2.00612458230316,31.5422973060038,1.15823656762066));
#7911=CARTESIAN_POINT('Ctrl Pts',(-2.00612458230317,31.4839639726704,0.));
#7912=CARTESIAN_POINT('Ctrl Pts',(-2.00612458230317,31.4256306393371,-1.15823656762066));
#7913=CARTESIAN_POINT('Ctrl Pts',(-1.00306229115158,31.3672973060038,-1.73735485143099));
#7914=CARTESIAN_POINT('Ctrl Pts',(-1.41843070519206E-16,31.3089639726704,
-2.31647313524132));
#7915=CARTESIAN_POINT('Ctrl Pts',(1.00306229115158,31.2506306393371,-1.73735485143099));
#7916=CARTESIAN_POINT('Ctrl Pts',(2.00612458230317,31.1922973060038,-1.15823656762066));
#7917=CARTESIAN_POINT('Ctrl Pts',(2.00612458230317,31.1339639726704,-2.45679404840839E-16));
#7918=CARTESIAN_POINT('Ctrl Pts',(2.00612458230317,31.0756306393371,1.15823656762066));
#7919=CARTESIAN_POINT('Ctrl Pts',(1.00306229115158,31.0172973060038,1.73735485143099));
#7920=CARTESIAN_POINT('Ctrl Pts',(4.25529211557617E-16,30.9589639726704,
2.31647313524132));
#7921=CARTESIAN_POINT('Ctrl Pts',(-1.00306229115158,30.9006306393371,1.73735485143099));
#7922=CARTESIAN_POINT('Ctrl Pts',(-2.00612458230316,30.8422973060038,1.15823656762066));
#7923=CARTESIAN_POINT('Ctrl Pts',(-2.00612458230317,30.7839639726704,0.));
#7924=CARTESIAN_POINT('Ctrl Pts',(-2.00612458230317,30.7256306393371,-1.15823656762066));
#7925=CARTESIAN_POINT('Ctrl Pts',(-1.00306229115158,30.6672973060038,-1.73735485143099));
#7926=CARTESIAN_POINT('Ctrl Pts',(-1.41843070519206E-16,30.6089639726704,
-2.31647313524132));
#7927=CARTESIAN_POINT('Ctrl Pts',(1.00306229115158,30.5506306393371,-1.73735485143099));
#7928=CARTESIAN_POINT('Ctrl Pts',(2.00612458230317,30.4922973060038,-1.15823656762066));
#7929=CARTESIAN_POINT('Ctrl Pts',(2.00612458230317,30.4339639726704,-2.45679404840839E-16));
#7930=CARTESIAN_POINT('Ctrl Pts',(2.00612458230317,30.3756306393371,1.15823656762066));
#7931=CARTESIAN_POINT('Ctrl Pts',(1.00306229115158,30.3172973060038,1.73735485143099));
#7932=CARTESIAN_POINT('Ctrl Pts',(4.25529211557617E-16,30.2589639726704,
2.31647313524132));
#7933=CARTESIAN_POINT('Ctrl Pts',(-1.00306229115158,30.2006306393371,1.73735485143099));
#7934=CARTESIAN_POINT('Ctrl Pts',(-2.00612458230316,30.1422973060038,1.15823656762066));
#7935=CARTESIAN_POINT('Ctrl Pts',(-2.00612458230317,30.0839639726704,0.));
#7936=CARTESIAN_POINT('Ctrl Pts',(-2.00612458230317,30.0256306393371,-1.15823656762066));
#7937=CARTESIAN_POINT('Ctrl Pts',(-1.00306229115158,29.9672973060038,-1.73735485143099));
#7938=CARTESIAN_POINT('Ctrl Pts',(-1.41843070519206E-16,29.9089639726704,
-2.31647313524132));
#7939=CARTESIAN_POINT('Ctrl Pts',(1.00306229115158,29.8506306393371,-1.73735485143099));
#7940=CARTESIAN_POINT('Ctrl Pts',(2.00612458230317,29.7922973060038,-1.15823656762066));
#7941=CARTESIAN_POINT('Ctrl Pts',(2.00612458230317,29.7339639726704,-2.45679404840839E-16));
#7942=CARTESIAN_POINT('Ctrl Pts',(2.00612458230317,29.6756306393371,1.15823656762066));
#7943=CARTESIAN_POINT('Ctrl Pts',(1.00306229115158,29.6172973060038,1.73735485143099));
#7944=CARTESIAN_POINT('Ctrl Pts',(4.25529211557617E-16,29.5589639726704,
2.31647313524132));
#7945=CARTESIAN_POINT('Ctrl Pts',(-1.00306229115158,29.5006306393371,1.73735485143099));
#7946=CARTESIAN_POINT('Ctrl Pts',(-2.00612458230316,29.4422973060038,1.15823656762066));
#7947=CARTESIAN_POINT('Ctrl Pts',(-2.00612458230317,29.3839639726704,0.));
#7948=CARTESIAN_POINT('Ctrl Pts',(-2.00612458230317,29.3256306393371,-1.15823656762066));
#7949=CARTESIAN_POINT('Ctrl Pts',(-1.00306229115158,29.2672973060038,-1.73735485143099));
#7950=CARTESIAN_POINT('Ctrl Pts',(-1.41843070519206E-16,29.2089639726704,
-2.31647313524132));
#7951=CARTESIAN_POINT('Ctrl Pts',(1.00306229115158,29.1506306393371,-1.73735485143099));
#7952=CARTESIAN_POINT('Ctrl Pts',(2.00612458230317,29.0922973060038,-1.15823656762066));
#7953=CARTESIAN_POINT('Ctrl Pts',(2.00612458230317,29.0339639726704,-2.45679404840839E-16));
#7954=CARTESIAN_POINT('Ctrl Pts',(2.00612458230317,28.9756306393371,1.15823656762066));
#7955=CARTESIAN_POINT('Ctrl Pts',(1.00306229115158,28.9172973060038,1.73735485143099));
#7956=CARTESIAN_POINT('Ctrl Pts',(4.25529211557617E-16,28.8589639726704,
2.31647313524132));
#7957=CARTESIAN_POINT('Ctrl Pts',(-1.00306229115158,28.8006306393371,1.73735485143099));
#7958=CARTESIAN_POINT('Ctrl Pts',(-2.00612458230316,28.7422973060038,1.15823656762066));
#7959=CARTESIAN_POINT('Ctrl Pts',(-2.00612458230317,28.6839639726704,0.));
#7960=CARTESIAN_POINT('Ctrl Pts',(-2.00612458230317,28.6256306393371,-1.15823656762066));
#7961=CARTESIAN_POINT('Ctrl Pts',(-1.00306229115158,28.5672973060038,-1.73735485143099));
#7962=CARTESIAN_POINT('Ctrl Pts',(-1.41843070519206E-16,28.5089639726704,
-2.31647313524132));
#7963=CARTESIAN_POINT('Ctrl Pts',(1.00306229115158,28.4506306393371,-1.73735485143099));
#7964=CARTESIAN_POINT('Ctrl Pts',(2.00612458230317,28.3922973060038,-1.15823656762066));
#7965=CARTESIAN_POINT('Ctrl Pts',(2.00612458230317,28.3339639726704,-2.45679404840839E-16));
#7966=CARTESIAN_POINT('Ctrl Pts',(2.00612458230317,28.2756306393371,1.15823656762066));
#7967=CARTESIAN_POINT('Ctrl Pts',(1.00306229115158,28.2172973060038,1.73735485143099));
#7968=CARTESIAN_POINT('Ctrl Pts',(4.25529211557617E-16,28.1589639726704,
2.31647313524132));
#7969=CARTESIAN_POINT('Ctrl Pts',(-1.00306229115158,28.1006306393371,1.73735485143099));
#7970=CARTESIAN_POINT('Ctrl Pts',(-2.00612458230316,28.0422973060038,1.15823656762066));
#7971=CARTESIAN_POINT('Ctrl Pts',(-2.00612458230317,27.9839639726704,0.));
#7972=CARTESIAN_POINT('Ctrl Pts',(-2.00612458230317,27.9256306393371,-1.15823656762066));
#7973=CARTESIAN_POINT('Ctrl Pts',(-1.00306229115158,27.8672973060038,-1.73735485143099));
#7974=CARTESIAN_POINT('Ctrl Pts',(-1.41843070519206E-16,27.8089639726704,
-2.31647313524132));
#7975=CARTESIAN_POINT('Ctrl Pts',(1.00306229115158,27.7506306393371,-1.73735485143099));
#7976=CARTESIAN_POINT('Ctrl Pts',(2.00612458230317,27.6922973060038,-1.15823656762066));
#7977=CARTESIAN_POINT('Ctrl Pts',(2.00612458230317,27.6339639726704,-2.45679404840839E-16));
#7978=CARTESIAN_POINT('Ctrl Pts',(2.00612458230317,27.5756306393371,1.15823656762066));
#7979=CARTESIAN_POINT('Ctrl Pts',(1.00306229115158,27.5172973060038,1.73735485143099));
#7980=CARTESIAN_POINT('Ctrl Pts',(4.25529211557617E-16,27.4589639726704,
2.31647313524132));
#7981=CARTESIAN_POINT('Ctrl Pts',(-1.00306229115158,27.4006306393371,1.73735485143099));
#7982=CARTESIAN_POINT('Ctrl Pts',(-2.00612458230316,27.3422973060038,1.15823656762066));
#7983=CARTESIAN_POINT('Ctrl Pts',(-2.00612458230317,27.2839639726704,0.));
#7984=CARTESIAN_POINT('Ctrl Pts',(-2.00612458230317,27.2256306393371,-1.15823656762066));
#7985=CARTESIAN_POINT('Ctrl Pts',(-1.00306229115158,27.1672973060038,-1.73735485143099));
#7986=CARTESIAN_POINT('Ctrl Pts',(-1.41843070519206E-16,27.1089639726704,
-2.31647313524132));
#7987=CARTESIAN_POINT('Ctrl Pts',(1.00306229115158,27.0506306393371,-1.73735485143099));
#7988=CARTESIAN_POINT('Ctrl Pts',(2.00612458230317,26.9922973060038,-1.15823656762066));
#7989=CARTESIAN_POINT('Ctrl Pts',(2.00612458230317,26.9339639726704,-2.45679404840839E-16));
#7990=CARTESIAN_POINT('Ctrl Pts',(2.00612458230317,26.8756306393371,1.15823656762066));
#7991=CARTESIAN_POINT('Ctrl Pts',(1.00306229115158,26.8172973060038,1.73735485143099));
#7992=CARTESIAN_POINT('Ctrl Pts',(4.25529211557617E-16,26.7589639726704,
2.31647313524132));
#7993=CARTESIAN_POINT('Ctrl Pts',(-1.00306229115158,26.7006306393371,1.73735485143099));
#7994=CARTESIAN_POINT('Ctrl Pts',(-2.00612458230316,26.6422973060038,1.15823656762066));
#7995=CARTESIAN_POINT('Ctrl Pts',(-2.00612458230317,26.5839639726704,0.));
#7996=CARTESIAN_POINT('Ctrl Pts',(-2.00612458230317,26.5256306393371,-1.15823656762066));
#7997=CARTESIAN_POINT('Ctrl Pts',(-1.00306229115158,26.4672973060038,-1.73735485143099));
#7998=CARTESIAN_POINT('Ctrl Pts',(-1.41843070519206E-16,26.4089639726704,
-2.31647313524132));
#7999=CARTESIAN_POINT('Ctrl Pts',(1.00306229115158,26.3506306393371,-1.73735485143099));
#8000=CARTESIAN_POINT('Ctrl Pts',(2.00612458230317,26.2922973060038,-1.15823656762066));
#8001=CARTESIAN_POINT('Ctrl Pts',(2.00612458230317,26.2339639726704,-2.45679404840839E-16));
#8002=CARTESIAN_POINT('Ctrl Pts',(2.00612458230317,26.1756306393371,1.15823656762066));
#8003=CARTESIAN_POINT('Ctrl Pts',(1.00306229115158,26.1172973060038,1.73735485143099));
#8004=CARTESIAN_POINT('Ctrl Pts',(4.25529211557617E-16,26.0589639726704,
2.31647313524132));
#8005=CARTESIAN_POINT('Ctrl Pts',(-1.00306229115158,26.0006306393371,1.73735485143099));
#8006=CARTESIAN_POINT('Ctrl Pts',(-2.00612458230316,25.9422973060038,1.15823656762066));
#8007=CARTESIAN_POINT('Ctrl Pts',(-2.00612458230317,25.8839639726704,0.));
#8008=CARTESIAN_POINT('Ctrl Pts',(-2.00612458230317,25.8256306393371,-1.15823656762066));
#8009=CARTESIAN_POINT('Ctrl Pts',(-1.00306229115158,25.7672973060038,-1.73735485143099));
#8010=CARTESIAN_POINT('Ctrl Pts',(-1.41843070519206E-16,25.7089639726704,
-2.31647313524132));
#8011=CARTESIAN_POINT('Ctrl Pts',(1.00306229115158,25.6506306393371,-1.73735485143099));
#8012=CARTESIAN_POINT('Ctrl Pts',(2.00612458230317,25.5922973060038,-1.15823656762066));
#8013=CARTESIAN_POINT('Ctrl Pts',(2.00612458230317,25.5339639726704,-2.45679404840839E-16));
#8014=CARTESIAN_POINT('Ctrl Pts',(2.00612458230317,25.4756306393371,1.15823656762066));
#8015=CARTESIAN_POINT('Ctrl Pts',(1.00306229115158,25.4172973060038,1.73735485143099));
#8016=CARTESIAN_POINT('Ctrl Pts',(4.25529211557617E-16,25.3589639726704,
2.31647313524132));
#8017=CARTESIAN_POINT('Ctrl Pts',(-1.00306229115158,25.3006306393371,1.73735485143099));
#8018=CARTESIAN_POINT('Ctrl Pts',(-2.00612458230316,25.2422973060038,1.15823656762066));
#8019=CARTESIAN_POINT('Ctrl Pts',(-2.00612458230317,25.1839639726704,0.));
#8020=CARTESIAN_POINT('Ctrl Pts',(-2.00612458230317,25.1256306393371,-1.15823656762066));
#8021=CARTESIAN_POINT('Ctrl Pts',(-1.00306229115158,25.0672973060038,-1.73735485143099));
#8022=CARTESIAN_POINT('Ctrl Pts',(-1.41843070519206E-16,25.0089639726704,
-2.31647313524132));
#8023=CARTESIAN_POINT('Ctrl Pts',(1.00306229115158,24.9506306393371,-1.73735485143099));
#8024=CARTESIAN_POINT('Ctrl Pts',(2.00612458230317,24.8922973060038,-1.15823656762066));
#8025=CARTESIAN_POINT('Ctrl Pts',(2.00612458230317,24.8339639726704,-2.45679404840839E-16));
#8026=CARTESIAN_POINT('Ctrl Pts',(2.00612458230317,24.7756306393371,1.15823656762066));
#8027=CARTESIAN_POINT('Ctrl Pts',(1.00306229115158,24.7172973060038,1.73735485143099));
#8028=CARTESIAN_POINT('Ctrl Pts',(4.25529211557617E-16,24.6589639726704,
2.31647313524132));
#8029=CARTESIAN_POINT('Ctrl Pts',(-1.00306229115158,24.6006306393371,1.73735485143099));
#8030=CARTESIAN_POINT('Ctrl Pts',(-2.00612458230316,24.5422973060038,1.15823656762066));
#8031=CARTESIAN_POINT('Ctrl Pts',(-2.00612458230317,24.4839639726704,0.));
#8032=CARTESIAN_POINT('Ctrl Pts',(-2.00612458230317,24.4256306393371,-1.15823656762066));
#8033=CARTESIAN_POINT('Ctrl Pts',(-1.00306229115158,24.3672973060038,-1.73735485143099));
#8034=CARTESIAN_POINT('Ctrl Pts',(-1.41843070519206E-16,24.3089639726704,
-2.31647313524132));
#8035=CARTESIAN_POINT('Ctrl Pts',(1.00306229115158,24.2506306393371,-1.73735485143099));
#8036=CARTESIAN_POINT('Ctrl Pts',(2.00612458230317,24.1922973060038,-1.15823656762066));
#8037=CARTESIAN_POINT('Ctrl Pts',(2.00612458230317,24.1339639726704,-2.45679404840839E-16));
#8038=CARTESIAN_POINT('Ctrl Pts',(2.00612458230317,24.0756306393371,1.15823656762066));
#8039=CARTESIAN_POINT('Ctrl Pts',(1.00306229115158,24.0172973060038,1.73735485143099));
#8040=CARTESIAN_POINT('Ctrl Pts',(4.25529211557617E-16,23.9589639726704,
2.31647313524132));
#8041=CARTESIAN_POINT('Ctrl Pts',(-1.00306229115158,23.9006306393371,1.73735485143099));
#8042=CARTESIAN_POINT('Ctrl Pts',(-2.00612458230316,23.8422973060038,1.15823656762066));
#8043=CARTESIAN_POINT('Ctrl Pts',(-2.00612458230317,23.7839639726704,0.));
#8044=CARTESIAN_POINT('Ctrl Pts',(-2.00612458230317,23.7256306393371,-1.15823656762066));
#8045=CARTESIAN_POINT('Ctrl Pts',(-1.00306229115158,23.6672973060038,-1.73735485143099));
#8046=CARTESIAN_POINT('Ctrl Pts',(-1.41843070519206E-16,23.6089639726704,
-2.31647313524132));
#8047=CARTESIAN_POINT('Ctrl Pts',(1.00306229115158,23.5506306393371,-1.73735485143099));
#8048=CARTESIAN_POINT('Ctrl Pts',(2.00612458230317,23.4922973060038,-1.15823656762066));
#8049=CARTESIAN_POINT('Ctrl Pts',(2.00612458230317,23.4339639726704,-2.45679404840839E-16));
#8050=CARTESIAN_POINT('Ctrl Pts',(2.00612458230317,23.3756306393371,1.15823656762066));
#8051=CARTESIAN_POINT('Ctrl Pts',(1.00306229115158,23.3172973060038,1.73735485143099));
#8052=CARTESIAN_POINT('Ctrl Pts',(4.25529211557617E-16,23.2589639726704,
2.31647313524132));
#8053=CARTESIAN_POINT('Ctrl Pts',(-1.00306229115158,23.2006306393371,1.73735485143099));
#8054=CARTESIAN_POINT('Ctrl Pts',(-2.00612458230316,23.1422973060038,1.15823656762066));
#8055=CARTESIAN_POINT('Ctrl Pts',(-2.00612458230317,23.0839639726704,0.));
#8056=CARTESIAN_POINT('Ctrl Pts',(-2.00612458230317,23.0256306393371,-1.15823656762066));
#8057=CARTESIAN_POINT('Ctrl Pts',(-1.00306229115158,22.9672973060038,-1.73735485143099));
#8058=CARTESIAN_POINT('Ctrl Pts',(-1.41843070519206E-16,22.9089639726704,
-2.31647313524132));
#8059=CARTESIAN_POINT('Ctrl Pts',(1.00306229115158,22.8506306393371,-1.73735485143099));
#8060=CARTESIAN_POINT('Ctrl Pts',(2.00612458230317,22.7922973060038,-1.15823656762066));
#8061=CARTESIAN_POINT('Ctrl Pts',(2.00612458230317,22.7339639726704,-2.45679404840839E-16));
#8062=CARTESIAN_POINT('Ctrl Pts',(2.00612458230317,22.6756306393371,1.15823656762066));
#8063=CARTESIAN_POINT('Ctrl Pts',(1.00306229115158,22.6172973060038,1.73735485143099));
#8064=CARTESIAN_POINT('Ctrl Pts',(4.25529211557617E-16,22.5589639726704,
2.31647313524132));
#8065=CARTESIAN_POINT('Ctrl Pts',(-1.00306229115158,22.5006306393371,1.73735485143099));
#8066=CARTESIAN_POINT('Ctrl Pts',(-2.00612458230316,22.4422973060038,1.15823656762066));
#8067=CARTESIAN_POINT('Ctrl Pts',(-2.00612458230317,22.3839639726704,0.));
#8068=CARTESIAN_POINT('Ctrl Pts',(-2.00612458230317,22.3256306393371,-1.15823656762066));
#8069=CARTESIAN_POINT('Ctrl Pts',(-1.00306229115158,22.2672973060038,-1.73735485143099));
#8070=CARTESIAN_POINT('Ctrl Pts',(-1.41843070519206E-16,22.2089639726704,
-2.31647313524132));
#8071=CARTESIAN_POINT('Ctrl Pts',(1.00306229115158,22.1506306393371,-1.73735485143099));
#8072=CARTESIAN_POINT('Ctrl Pts',(2.00612458230317,22.0922973060038,-1.15823656762066));
#8073=CARTESIAN_POINT('Ctrl Pts',(2.00612458230317,22.0339639726704,-2.45679404840839E-16));
#8074=CARTESIAN_POINT('Ctrl Pts',(2.00612458230317,21.9756306393371,1.15823656762066));
#8075=CARTESIAN_POINT('Ctrl Pts',(1.00306229115158,21.9172973060038,1.73735485143099));
#8076=CARTESIAN_POINT('Ctrl Pts',(4.25529211557617E-16,21.8589639726704,
2.31647313524132));
#8077=CARTESIAN_POINT('Ctrl Pts',(-1.00306229115158,21.8006306393371,1.73735485143099));
#8078=CARTESIAN_POINT('Ctrl Pts',(-2.00612458230316,21.7422973060038,1.15823656762066));
#8079=CARTESIAN_POINT('Ctrl Pts',(-2.00612458230317,21.6839639726704,0.));
#8080=CARTESIAN_POINT('Ctrl Pts',(-2.00612458230317,21.6256306393371,-1.15823656762066));
#8081=CARTESIAN_POINT('Ctrl Pts',(-1.00306229115158,21.5672973060038,-1.73735485143099));
#8082=CARTESIAN_POINT('Ctrl Pts',(-1.41843070519206E-16,21.5089639726704,
-2.31647313524132));
#8083=CARTESIAN_POINT('Ctrl Pts',(1.00306229115158,21.4506306393371,-1.73735485143099));
#8084=CARTESIAN_POINT('Ctrl Pts',(2.00612458230317,21.3922973060038,-1.15823656762066));
#8085=CARTESIAN_POINT('Ctrl Pts',(2.00612458230317,21.3339639726704,-2.45679404840839E-16));
#8086=CARTESIAN_POINT('Ctrl Pts',(2.00612458230317,21.2756306393371,1.15823656762066));
#8087=CARTESIAN_POINT('Ctrl Pts',(1.00306229115158,21.2172973060038,1.73735485143099));
#8088=CARTESIAN_POINT('Ctrl Pts',(4.25529211557617E-16,21.1589639726704,
2.31647313524132));
#8089=CARTESIAN_POINT('Ctrl Pts',(-1.00306229115158,21.1006306393371,1.73735485143099));
#8090=CARTESIAN_POINT('Ctrl Pts',(-2.00612458230316,21.0422973060038,1.15823656762066));
#8091=CARTESIAN_POINT('Ctrl Pts',(-2.00612458230317,20.9839639726704,0.));
#8092=CARTESIAN_POINT('Ctrl Pts',(-2.00612458230317,20.9256306393371,-1.15823656762066));
#8093=CARTESIAN_POINT('Ctrl Pts',(-1.00306229115158,20.8672973060038,-1.73735485143099));
#8094=CARTESIAN_POINT('Ctrl Pts',(-1.41843070519206E-16,20.8089639726704,
-2.31647313524132));
#8095=CARTESIAN_POINT('Ctrl Pts',(1.00306229115158,20.7506306393371,-1.73735485143099));
#8096=CARTESIAN_POINT('Ctrl Pts',(2.00612458230317,20.6922973060038,-1.15823656762066));
#8097=CARTESIAN_POINT('Ctrl Pts',(2.00612458230317,20.6339639726704,-2.45679404840839E-16));
#8098=CARTESIAN_POINT('Ctrl Pts',(2.00612458230317,20.5756306393371,1.15823656762066));
#8099=CARTESIAN_POINT('Ctrl Pts',(1.00306229115158,20.5172973060038,1.73735485143099));
#8100=CARTESIAN_POINT('Ctrl Pts',(4.25529211557617E-16,20.4589639726704,
2.31647313524132));
#8101=CARTESIAN_POINT('Ctrl Pts',(-1.00306229115158,20.4006306393371,1.73735485143099));
#8102=CARTESIAN_POINT('Ctrl Pts',(-2.00612458230316,20.3422973060038,1.15823656762066));
#8103=CARTESIAN_POINT('Ctrl Pts',(-2.00612458230317,20.2839639726704,0.));
#8104=CARTESIAN_POINT('Ctrl Pts',(-2.00612458230317,20.2256306393371,-1.15823656762066));
#8105=CARTESIAN_POINT('Ctrl Pts',(-1.00306229115158,20.1672973060038,-1.73735485143099));
#8106=CARTESIAN_POINT('Ctrl Pts',(-1.41843070519206E-16,20.1089639726704,
-2.31647313524132));
#8107=CARTESIAN_POINT('Ctrl Pts',(1.00306229115158,20.0506306393371,-1.73735485143099));
#8108=CARTESIAN_POINT('Ctrl Pts',(2.00612458230317,19.9922973060038,-1.15823656762066));
#8109=CARTESIAN_POINT('Ctrl Pts',(2.00612458230317,19.9339639726704,-2.45679404840839E-16));
#8110=CARTESIAN_POINT('Ctrl Pts',(2.00612458230317,19.8756306393371,1.15823656762066));
#8111=CARTESIAN_POINT('Ctrl Pts',(1.00306229115158,19.8172973060038,1.73735485143099));
#8112=CARTESIAN_POINT('Ctrl Pts',(4.25529211557617E-16,19.7589639726704,
2.31647313524132));
#8113=CARTESIAN_POINT('Ctrl Pts',(-1.00306229115158,19.7006306393371,1.73735485143099));
#8114=CARTESIAN_POINT('Ctrl Pts',(-2.00612458230316,19.6422973060038,1.15823656762066));
#8115=CARTESIAN_POINT('Ctrl Pts',(-2.00612458230317,19.5839639726704,0.));
#8116=CARTESIAN_POINT('Ctrl Pts',(-2.00612458230317,19.5256306393371,-1.15823656762066));
#8117=CARTESIAN_POINT('Ctrl Pts',(-1.00306229115158,19.4672973060038,-1.73735485143099));
#8118=CARTESIAN_POINT('Ctrl Pts',(-1.41843070519206E-16,19.4089639726704,
-2.31647313524132));
#8119=CARTESIAN_POINT('Ctrl Pts',(1.00306229115158,19.3506306393371,-1.73735485143099));
#8120=CARTESIAN_POINT('Ctrl Pts',(2.00612458230317,19.2922973060038,-1.15823656762066));
#8121=CARTESIAN_POINT('Ctrl Pts',(2.00612458230317,19.2339639726704,-2.45679404840839E-16));
#8122=CARTESIAN_POINT('Ctrl Pts',(2.00612458230317,19.1756306393371,1.15823656762066));
#8123=CARTESIAN_POINT('Ctrl Pts',(1.00306229115158,19.1172973060038,1.73735485143099));
#8124=CARTESIAN_POINT('Ctrl Pts',(4.25529211557617E-16,19.0589639726704,
2.31647313524132));
#8125=CARTESIAN_POINT('Ctrl Pts',(-1.00306229115158,19.0006306393371,1.73735485143099));
#8126=CARTESIAN_POINT('Ctrl Pts',(-2.00612458230316,18.9422973060038,1.15823656762066));
#8127=CARTESIAN_POINT('Ctrl Pts',(-2.00612458230317,18.8839639726704,0.));
#8128=CARTESIAN_POINT('Ctrl Pts',(-2.00612458230317,18.8256306393371,-1.15823656762066));
#8129=CARTESIAN_POINT('Ctrl Pts',(-1.00306229115158,18.7672973060038,-1.73735485143099));
#8130=CARTESIAN_POINT('Ctrl Pts',(-1.41843070519206E-16,18.7089639726704,
-2.31647313524132));
#8131=CARTESIAN_POINT('Ctrl Pts',(1.00306229115158,18.6506306393371,-1.73735485143099));
#8132=CARTESIAN_POINT('Ctrl Pts',(2.00612458230317,18.5922973060038,-1.15823656762066));
#8133=CARTESIAN_POINT('Ctrl Pts',(2.00612458230317,18.5339639726704,-2.45679404840839E-16));
#8134=CARTESIAN_POINT('Ctrl Pts',(2.00612458230317,18.4756306393371,1.15823656762066));
#8135=CARTESIAN_POINT('Ctrl Pts',(1.00306229115158,18.4172973060038,1.73735485143099));
#8136=CARTESIAN_POINT('Ctrl Pts',(4.25529211557617E-16,18.3589639726704,
2.31647313524132));
#8137=CARTESIAN_POINT('Ctrl Pts',(-1.00306229115158,18.3006306393371,1.73735485143099));
#8138=CARTESIAN_POINT('Ctrl Pts',(-2.00612458230316,18.2422973060038,1.15823656762066));
#8139=CARTESIAN_POINT('Ctrl Pts',(-2.00612458230317,18.1839639726704,0.));
#8140=CARTESIAN_POINT('Ctrl Pts',(-2.00612458230317,18.1256306393371,-1.15823656762066));
#8141=CARTESIAN_POINT('Ctrl Pts',(-1.00306229115158,18.0672973060038,-1.73735485143099));
#8142=CARTESIAN_POINT('Ctrl Pts',(-1.41843070519206E-16,18.0089639726704,
-2.31647313524132));
#8143=CARTESIAN_POINT('Ctrl Pts',(1.00306229115158,17.9506306393371,-1.73735485143099));
#8144=CARTESIAN_POINT('Ctrl Pts',(2.00612458230317,17.8922973060038,-1.15823656762066));
#8145=CARTESIAN_POINT('Ctrl Pts',(2.00612458230317,17.8339639726704,-2.45679404840839E-16));
#8146=CARTESIAN_POINT('Ctrl Pts',(2.00612458230317,17.7756306393371,1.15823656762066));
#8147=CARTESIAN_POINT('Ctrl Pts',(1.00306229115158,17.7172973060038,1.73735485143099));
#8148=CARTESIAN_POINT('Ctrl Pts',(4.25529211557617E-16,17.6589639726704,
2.31647313524132));
#8149=CARTESIAN_POINT('Ctrl Pts',(-1.00306229115158,17.6006306393371,1.73735485143099));
#8150=CARTESIAN_POINT('Ctrl Pts',(-2.00612458230316,17.5422973060038,1.15823656762066));
#8151=CARTESIAN_POINT('Ctrl Pts',(-2.00612458230317,17.4839639726704,0.));
#8152=CARTESIAN_POINT('Ctrl Pts',(-2.00612458230317,17.4256306393371,-1.15823656762066));
#8153=CARTESIAN_POINT('Ctrl Pts',(-1.00306229115158,17.3672973060038,-1.73735485143099));
#8154=CARTESIAN_POINT('Ctrl Pts',(-1.41843070519206E-16,17.3089639726704,
-2.31647313524132));
#8155=CARTESIAN_POINT('Ctrl Pts',(1.00306229115158,17.2506306393371,-1.73735485143099));
#8156=CARTESIAN_POINT('Ctrl Pts',(2.00612458230317,17.1922973060038,-1.15823656762066));
#8157=CARTESIAN_POINT('Ctrl Pts',(2.00612458230317,17.1339639726704,-2.45679404840839E-16));
#8158=CARTESIAN_POINT('Ctrl Pts',(2.00612458230317,17.0756306393371,1.15823656762066));
#8159=CARTESIAN_POINT('Ctrl Pts',(1.00306229115158,17.0172973060038,1.73735485143099));
#8160=CARTESIAN_POINT('Ctrl Pts',(4.25529211557617E-16,16.9589639726704,
2.31647313524132));
#8161=CARTESIAN_POINT('Ctrl Pts',(-1.00306229115158,16.9006306393371,1.73735485143099));
#8162=CARTESIAN_POINT('Ctrl Pts',(-2.00612458230316,16.8422973060038,1.15823656762066));
#8163=CARTESIAN_POINT('Ctrl Pts',(-2.00612458230317,16.7839639726704,0.));
#8164=CARTESIAN_POINT('Ctrl Pts',(-2.00612458230317,16.7256306393371,-1.15823656762066));
#8165=CARTESIAN_POINT('Ctrl Pts',(-1.00306229115158,16.6672973060038,-1.73735485143099));
#8166=CARTESIAN_POINT('Ctrl Pts',(-1.41843070519206E-16,16.6089639726704,
-2.31647313524132));
#8167=CARTESIAN_POINT('Ctrl Pts',(1.00306229115158,16.5506306393371,-1.73735485143099));
#8168=CARTESIAN_POINT('Ctrl Pts',(2.00612458230317,16.4922973060038,-1.15823656762066));
#8169=CARTESIAN_POINT('Ctrl Pts',(2.00612458230317,16.4339639726704,-2.45679404840839E-16));
#8170=CARTESIAN_POINT('Ctrl Pts',(2.00612458230317,16.3756306393371,1.15823656762066));
#8171=CARTESIAN_POINT('Ctrl Pts',(1.00306229115158,16.3172973060038,1.73735485143099));
#8172=CARTESIAN_POINT('Ctrl Pts',(4.25529211557617E-16,16.2589639726704,
2.31647313524132));
#8173=CARTESIAN_POINT('Ctrl Pts',(-1.00306229115158,16.2006306393371,1.73735485143099));
#8174=CARTESIAN_POINT('Ctrl Pts',(-2.00612458230316,16.1422973060038,1.15823656762066));
#8175=CARTESIAN_POINT('Ctrl Pts',(-2.00612458230317,16.0839639726704,0.));
#8176=CARTESIAN_POINT('Ctrl Pts',(-2.00612458230317,16.0256306393371,-1.15823656762066));
#8177=CARTESIAN_POINT('Ctrl Pts',(-1.00306229115158,15.9672973060038,-1.73735485143099));
#8178=CARTESIAN_POINT('Ctrl Pts',(-1.41843070519206E-16,15.9089639726704,
-2.31647313524132));
#8179=CARTESIAN_POINT('Ctrl Pts',(1.00306229115158,15.8506306393371,-1.73735485143099));
#8180=CARTESIAN_POINT('Ctrl Pts',(2.00612458230317,15.7922973060038,-1.15823656762066));
#8181=CARTESIAN_POINT('Ctrl Pts',(2.00612458230317,15.7339639726704,-2.45679404840839E-16));
#8182=CARTESIAN_POINT('Ctrl Pts',(2.00612458230317,15.6756306393371,1.15823656762066));
#8183=CARTESIAN_POINT('Ctrl Pts',(1.00306229115158,15.6172973060038,1.73735485143099));
#8184=CARTESIAN_POINT('Ctrl Pts',(4.25529211557617E-16,15.5589639726704,
2.31647313524132));
#8185=CARTESIAN_POINT('Ctrl Pts',(-1.00306229115158,15.5006306393371,1.73735485143099));
#8186=CARTESIAN_POINT('Ctrl Pts',(-2.00612458230316,15.4422973060038,1.15823656762066));
#8187=CARTESIAN_POINT('Ctrl Pts',(-2.00612458230317,15.3839639726704,0.));
#8188=CARTESIAN_POINT('Ctrl Pts',(-2.00612458230317,15.3256306393371,-1.15823656762066));
#8189=CARTESIAN_POINT('Ctrl Pts',(-1.00306229115158,15.2672973060038,-1.73735485143099));
#8190=CARTESIAN_POINT('Ctrl Pts',(-1.41843070519206E-16,15.2089639726704,
-2.31647313524132));
#8191=CARTESIAN_POINT('Ctrl Pts',(1.00306229115158,15.1506306393371,-1.73735485143099));
#8192=CARTESIAN_POINT('Ctrl Pts',(2.00612458230317,15.0922973060038,-1.15823656762066));
#8193=CARTESIAN_POINT('Ctrl Pts',(2.00612458230317,15.0339639726704,-2.45679404840839E-16));
#8194=CARTESIAN_POINT('Ctrl Pts',(2.00612458230317,14.9756306393371,1.15823656762066));
#8195=CARTESIAN_POINT('Ctrl Pts',(1.00306229115158,14.9172973060038,1.73735485143099));
#8196=CARTESIAN_POINT('Ctrl Pts',(4.25529211557617E-16,14.8589639726704,
2.31647313524132));
#8197=CARTESIAN_POINT('Ctrl Pts',(-1.00306229115158,14.8006306393371,1.73735485143099));
#8198=CARTESIAN_POINT('Ctrl Pts',(-2.00612458230316,14.7422973060038,1.15823656762066));
#8199=CARTESIAN_POINT('Ctrl Pts',(-2.00612458230317,14.6839639726704,0.));
#8200=CARTESIAN_POINT('Ctrl Pts',(-2.00612458230317,14.6256306393371,-1.15823656762066));
#8201=CARTESIAN_POINT('Ctrl Pts',(-1.00306229115158,14.5672973060038,-1.73735485143099));
#8202=CARTESIAN_POINT('Ctrl Pts',(-1.41843070519206E-16,14.5089639726704,
-2.31647313524132));
#8203=CARTESIAN_POINT('Ctrl Pts',(1.00306229115158,14.4506306393371,-1.73735485143099));
#8204=CARTESIAN_POINT('Ctrl Pts',(2.00612458230317,14.3922973060038,-1.15823656762066));
#8205=CARTESIAN_POINT('Ctrl Pts',(2.00612458230317,14.3339639726704,-2.45679404840839E-16));
#8206=CARTESIAN_POINT('Ctrl Pts',(2.00612458230317,14.2756306393371,1.15823656762066));
#8207=CARTESIAN_POINT('Ctrl Pts',(1.00306229115158,14.2172973060038,1.73735485143099));
#8208=CARTESIAN_POINT('Ctrl Pts',(4.25529211557617E-16,14.1589639726704,
2.31647313524132));
#8209=CARTESIAN_POINT('Ctrl Pts',(-1.00306229115158,14.1006306393371,1.73735485143099));
#8210=CARTESIAN_POINT('Ctrl Pts',(-2.00612458230316,14.0422973060038,1.15823656762066));
#8211=CARTESIAN_POINT('Ctrl Pts',(-2.00612458230317,13.9839639726704,0.));
#8212=CARTESIAN_POINT('Ctrl Pts',(-2.00612458230317,13.9256306393371,-1.15823656762066));
#8213=CARTESIAN_POINT('Ctrl Pts',(-1.00306229115158,13.8672973060038,-1.73735485143099));
#8214=CARTESIAN_POINT('Ctrl Pts',(-1.41843070519206E-16,13.8089639726704,
-2.31647313524132));
#8215=CARTESIAN_POINT('Ctrl Pts',(1.00306229115158,13.7506306393371,-1.73735485143099));
#8216=CARTESIAN_POINT('Ctrl Pts',(2.00612458230317,13.6922973060038,-1.15823656762066));
#8217=CARTESIAN_POINT('Ctrl Pts',(2.00612458230317,13.6339639726704,-2.45679404840839E-16));
#8218=CARTESIAN_POINT('Ctrl Pts',(2.00612458230317,13.5756306393371,1.15823656762066));
#8219=CARTESIAN_POINT('Ctrl Pts',(1.00306229115158,13.5172973060038,1.73735485143099));
#8220=CARTESIAN_POINT('Ctrl Pts',(4.25529211557617E-16,13.4589639726704,
2.31647313524132));
#8221=CARTESIAN_POINT('Ctrl Pts',(-1.00306229115158,13.4006306393371,1.73735485143099));
#8222=CARTESIAN_POINT('Ctrl Pts',(-2.00612458230316,13.3422973060038,1.15823656762066));
#8223=CARTESIAN_POINT('Ctrl Pts',(-2.00612458230317,13.2839639726704,0.));
#8224=CARTESIAN_POINT('Ctrl Pts',(-2.00612458230317,13.2256306393371,-1.15823656762066));
#8225=CARTESIAN_POINT('Ctrl Pts',(-1.00306229115158,13.1672973060038,-1.73735485143099));
#8226=CARTESIAN_POINT('Ctrl Pts',(-1.41843070519206E-16,13.1089639726704,
-2.31647313524132));
#8227=CARTESIAN_POINT('Ctrl Pts',(1.00306229115158,13.0506306393371,-1.73735485143099));
#8228=CARTESIAN_POINT('Ctrl Pts',(2.00612458230317,12.9922973060038,-1.15823656762066));
#8229=CARTESIAN_POINT('Ctrl Pts',(2.00612458230317,12.9339639726704,-2.45679404840839E-16));
#8230=CARTESIAN_POINT('Ctrl Pts',(2.00612458230317,12.8756306393371,1.15823656762066));
#8231=CARTESIAN_POINT('Ctrl Pts',(1.00306229115158,12.8172973060038,1.73735485143099));
#8232=CARTESIAN_POINT('Ctrl Pts',(4.25529211557617E-16,12.7589639726704,
2.31647313524132));
#8233=CARTESIAN_POINT('Ctrl Pts',(-1.00306229115158,12.7006306393371,1.73735485143099));
#8234=CARTESIAN_POINT('Ctrl Pts',(-2.00612458230316,12.6422973060038,1.15823656762066));
#8235=CARTESIAN_POINT('Ctrl Pts',(-2.00612458230317,12.5839639726704,0.));
#8236=CARTESIAN_POINT('Ctrl Pts',(-2.00612458230317,12.5256306393371,-1.15823656762066));
#8237=CARTESIAN_POINT('Ctrl Pts',(-1.00306229115158,12.4672973060038,-1.73735485143099));
#8238=CARTESIAN_POINT('Ctrl Pts',(-1.41843070519206E-16,12.4089639726704,
-2.31647313524132));
#8239=CARTESIAN_POINT('Ctrl Pts',(1.00306229115158,12.3506306393371,-1.73735485143099));
#8240=CARTESIAN_POINT('Ctrl Pts',(2.00612458230317,12.2922973060038,-1.15823656762066));
#8241=CARTESIAN_POINT('Ctrl Pts',(2.00612458230317,12.2339639726704,-2.45679404840839E-16));
#8242=CARTESIAN_POINT('Ctrl Pts',(2.00612458230317,12.1756306393371,1.15823656762066));
#8243=CARTESIAN_POINT('Ctrl Pts',(1.00306229115158,12.1172973060038,1.73735485143099));
#8244=CARTESIAN_POINT('Ctrl Pts',(4.25529211557617E-16,12.0589639726704,
2.31647313524132));
#8245=CARTESIAN_POINT('Ctrl Pts',(-1.00306229115158,12.0006306393371,1.73735485143099));
#8246=CARTESIAN_POINT('Ctrl Pts',(-2.00612458230316,11.9422973060038,1.15823656762066));
#8247=CARTESIAN_POINT('Ctrl Pts',(-2.00612458230317,11.8839639726704,0.));
#8248=CARTESIAN_POINT('Ctrl Pts',(-2.00612458230317,11.8256306393371,-1.15823656762066));
#8249=CARTESIAN_POINT('Ctrl Pts',(-1.00306229115158,11.7672973060038,-1.73735485143099));
#8250=CARTESIAN_POINT('Ctrl Pts',(-1.41843070519206E-16,11.7089639726704,
-2.31647313524132));
#8251=CARTESIAN_POINT('Ctrl Pts',(1.00306229115158,11.6506306393371,-1.73735485143099));
#8252=CARTESIAN_POINT('Ctrl Pts',(2.00612458230317,11.5922973060038,-1.15823656762066));
#8253=CARTESIAN_POINT('Ctrl Pts',(2.00612458230317,11.5339639726704,-2.45679404840839E-16));
#8254=CARTESIAN_POINT('Ctrl Pts',(2.00612458230317,11.4756306393371,1.15823656762066));
#8255=CARTESIAN_POINT('Ctrl Pts',(1.00306229115158,11.4172973060038,1.73735485143099));
#8256=CARTESIAN_POINT('Ctrl Pts',(4.25529211557617E-16,11.3589639726704,
2.31647313524132));
#8257=CARTESIAN_POINT('Ctrl Pts',(-1.00306229115158,11.3006306393371,1.73735485143099));
#8258=CARTESIAN_POINT('Ctrl Pts',(-2.00612458230316,11.2422973060038,1.15823656762066));
#8259=CARTESIAN_POINT('Ctrl Pts',(-2.00612458230317,11.1839639726704,0.));
#8260=CARTESIAN_POINT('Ctrl Pts',(-2.00612458230317,11.1256306393371,-1.15823656762066));
#8261=CARTESIAN_POINT('Ctrl Pts',(-1.00306229115158,11.0672973060038,-1.73735485143099));
#8262=CARTESIAN_POINT('Ctrl Pts',(-1.41843070519206E-16,11.0089639726704,
-2.31647313524132));
#8263=CARTESIAN_POINT('Ctrl Pts',(1.00306229115158,10.9506306393371,-1.73735485143099));
#8264=CARTESIAN_POINT('Ctrl Pts',(2.00612458230317,10.8922973060038,-1.15823656762066));
#8265=CARTESIAN_POINT('Ctrl Pts',(2.00612458230317,10.8339639726704,-2.45679404840839E-16));
#8266=CARTESIAN_POINT('Ctrl Pts',(2.00612458230317,10.7756306393371,1.15823656762066));
#8267=CARTESIAN_POINT('Ctrl Pts',(1.00306229115158,10.7172973060038,1.73735485143099));
#8268=CARTESIAN_POINT('Ctrl Pts',(4.25529211557617E-16,10.6589639726704,
2.31647313524132));
#8269=CARTESIAN_POINT('Ctrl Pts',(-1.00306229115158,10.6006306393371,1.73735485143099));
#8270=CARTESIAN_POINT('Ctrl Pts',(-2.00612458230316,10.5422973060038,1.15823656762066));
#8271=CARTESIAN_POINT('Ctrl Pts',(-2.00612458230317,10.4839639726704,0.));
#8272=CARTESIAN_POINT('Ctrl Pts',(-2.00612458230317,10.4256306393371,-1.15823656762066));
#8273=CARTESIAN_POINT('Ctrl Pts',(-1.00306229115158,10.3672973060038,-1.73735485143099));
#8274=CARTESIAN_POINT('Ctrl Pts',(-1.41843070519206E-16,10.3089639726704,
-2.31647313524132));
#8275=CARTESIAN_POINT('Ctrl Pts',(1.00306229115158,10.2506306393371,-1.73735485143099));
#8276=CARTESIAN_POINT('Ctrl Pts',(2.00612458230317,10.1922973060038,-1.15823656762066));
#8277=CARTESIAN_POINT('Ctrl Pts',(2.00612458230317,10.1339639726704,-2.45679404840839E-16));
#8278=CARTESIAN_POINT('Ctrl Pts',(2.00612458230317,10.0756306393371,1.15823656762066));
#8279=CARTESIAN_POINT('Ctrl Pts',(1.00306229115158,10.0172973060038,1.73735485143099));
#8280=CARTESIAN_POINT('Ctrl Pts',(4.25529211557617E-16,9.95896397267043,
2.31647313524132));
#8281=CARTESIAN_POINT('Ctrl Pts',(-1.00306229115158,9.9006306393371,1.73735485143099));
#8282=CARTESIAN_POINT('Ctrl Pts',(-2.00612458230316,9.84229730600376,1.15823656762066));
#8283=CARTESIAN_POINT('Ctrl Pts',(-2.00612458230317,9.78396397267043,0.));
#8284=CARTESIAN_POINT('Ctrl Pts',(-2.00612458230317,9.7256306393371,-1.15823656762066));
#8285=CARTESIAN_POINT('Ctrl Pts',(-1.00306229115158,9.66729730600377,-1.73735485143099));
#8286=CARTESIAN_POINT('Ctrl Pts',(-1.41843070519206E-16,9.60896397267043,
-2.31647313524132));
#8287=CARTESIAN_POINT('Ctrl Pts',(1.00306229115158,9.5506306393371,-1.73735485143099));
#8288=CARTESIAN_POINT('Ctrl Pts',(2.00612458230317,9.49229730600377,-1.15823656762066));
#8289=CARTESIAN_POINT('Ctrl Pts',(2.00612458230317,9.43396397267043,-2.45679404840839E-16));
#8290=CARTESIAN_POINT('Ctrl Pts',(2.00612458230317,9.3756306393371,1.15823656762066));
#8291=CARTESIAN_POINT('Ctrl Pts',(1.00306229115158,9.31729730600377,1.73735485143099));
#8292=CARTESIAN_POINT('Ctrl Pts',(4.25529211557617E-16,9.25896397267043,
2.31647313524132));
#8293=CARTESIAN_POINT('Ctrl Pts',(-1.00306229115158,9.2006306393371,1.73735485143099));
#8294=CARTESIAN_POINT('Ctrl Pts',(-2.00612458230316,9.14229730600376,1.15823656762066));
#8295=CARTESIAN_POINT('Ctrl Pts',(-2.00612458230317,9.08396397267043,0.));
#8296=CARTESIAN_POINT('Ctrl Pts',(-2.00612458230317,9.0256306393371,-1.15823656762066));
#8297=CARTESIAN_POINT('Ctrl Pts',(-1.00306229115158,8.96729730600376,-1.73735485143099));
#8298=CARTESIAN_POINT('Ctrl Pts',(-1.41843070519206E-16,8.90896397267043,
-2.31647313524132));
#8299=CARTESIAN_POINT('Ctrl Pts',(1.00306229115158,8.8506306393371,-1.73735485143099));
#8300=CARTESIAN_POINT('Ctrl Pts',(2.00612458230317,8.79229730600376,-1.15823656762066));
#8301=CARTESIAN_POINT('Ctrl Pts',(2.00612458230317,8.73396397267044,-2.45679404840839E-16));
#8302=CARTESIAN_POINT('Ctrl Pts',(2.00612458230317,8.67563063933709,1.15823656762066));
#8303=CARTESIAN_POINT('Ctrl Pts',(1.00306229115158,8.61729730600377,1.73735485143099));
#8304=CARTESIAN_POINT('Ctrl Pts',(4.25529211557617E-16,8.55896397267043,
2.31647313524132));
#8305=CARTESIAN_POINT('Ctrl Pts',(-1.00306229115158,8.5006306393371,1.73735485143099));
#8306=CARTESIAN_POINT('Ctrl Pts',(-2.00612458230316,8.44229730600377,1.15823656762066));
#8307=CARTESIAN_POINT('Ctrl Pts',(-2.00612458230317,8.38396397267043,0.));
#8308=CARTESIAN_POINT('Ctrl Pts',(-2.00612458230317,8.3256306393371,-1.15823656762066));
#8309=CARTESIAN_POINT('Ctrl Pts',(-1.00306229115158,8.26729730600376,-1.73735485143099));
#8310=CARTESIAN_POINT('Ctrl Pts',(-1.41843070519206E-16,8.20896397267044,
-2.31647313524132));
#8311=CARTESIAN_POINT('Ctrl Pts',(1.00306229115158,8.1506306393371,-1.73735485143099));
#8312=CARTESIAN_POINT('Ctrl Pts',(2.00612458230317,8.09229730600377,-1.15823656762066));
#8313=CARTESIAN_POINT('Ctrl Pts',(2.00612458230317,8.03396397267043,-2.45679404840839E-16));
#8314=CARTESIAN_POINT('Ctrl Pts',(2.00612458230317,7.9756306393371,1.15823656762066));
#8315=CARTESIAN_POINT('Ctrl Pts',(1.00306229115158,7.91729730600376,1.73735485143099));
#8316=CARTESIAN_POINT('Ctrl Pts',(4.25529211557617E-16,7.85896397267043,
2.31647313524132));
#8317=CARTESIAN_POINT('Ctrl Pts',(-1.00306229115158,7.80063063933709,1.73735485143099));
#8318=CARTESIAN_POINT('Ctrl Pts',(-2.00612458230316,7.74229730600377,1.15823656762066));
#8319=CARTESIAN_POINT('Ctrl Pts',(-2.00612458230317,7.68396397267044,0.));
#8320=CARTESIAN_POINT('Ctrl Pts',(-2.00612458230317,7.6256306393371,-1.15823656762066));
#8321=CARTESIAN_POINT('Ctrl Pts',(-1.00306229115158,7.56729730600377,-1.73735485143099));
#8322=CARTESIAN_POINT('Ctrl Pts',(-1.41843070519206E-16,7.50896397267043,
-2.31647313524132));
#8323=CARTESIAN_POINT('Ctrl Pts',(1.00306229115158,7.4506306393371,-1.73735485143099));
#8324=CARTESIAN_POINT('Ctrl Pts',(2.00612458230317,7.39229730600376,-1.15823656762066));
#8325=CARTESIAN_POINT('Ctrl Pts',(2.00612458230317,7.33396397267044,-2.45679404840839E-16));
#8326=CARTESIAN_POINT('Ctrl Pts',(2.00612458230317,7.2756306393371,1.15823656762066));
#8327=CARTESIAN_POINT('Ctrl Pts',(1.00306229115158,7.21729730600377,1.73735485143099));
#8328=CARTESIAN_POINT('Ctrl Pts',(4.25529211557617E-16,7.15896397267043,
2.31647313524132));
#8329=CARTESIAN_POINT('Ctrl Pts',(-1.00306229115158,7.1006306393371,1.73735485143099));
#8330=CARTESIAN_POINT('Ctrl Pts',(-2.00612458230316,7.04229730600376,1.15823656762066));
#8331=CARTESIAN_POINT('Ctrl Pts',(-2.00612458230317,6.98396397267043,0.));
#8332=CARTESIAN_POINT('Ctrl Pts',(-2.00612458230317,6.92563063933711,-1.15823656762066));
#8333=CARTESIAN_POINT('Ctrl Pts',(-1.00306229115158,6.86729730600377,-1.73735485143099));
#8334=CARTESIAN_POINT('Ctrl Pts',(-1.41843070519206E-16,6.80896397267044,
-2.31647313524132));
#8335=CARTESIAN_POINT('Ctrl Pts',(1.00306229115158,6.7506306393371,-1.73735485143099));
#8336=CARTESIAN_POINT('Ctrl Pts',(2.00612458230317,6.69229730600377,-1.15823656762066));
#8337=CARTESIAN_POINT('Ctrl Pts',(2.00612458230317,6.63396397267043,-2.45679404840839E-16));
#8338=CARTESIAN_POINT('Ctrl Pts',(2.00612458230317,6.5756306393371,1.15823656762066));
#8339=CARTESIAN_POINT('Ctrl Pts',(1.00306229115158,6.51729730600376,1.73735485143099));
#8340=CARTESIAN_POINT('Ctrl Pts',(4.25529211557617E-16,6.45896397267044,
2.31647313524132));
#8341=CARTESIAN_POINT('Ctrl Pts',(-1.00306229115158,6.4006306393371,1.73735485143099));
#8342=CARTESIAN_POINT('Ctrl Pts',(-2.00612458230316,6.34229730600377,1.15823656762066));
#8343=CARTESIAN_POINT('Ctrl Pts',(-2.00612458230317,6.28396397267043,0.));
#8344=CARTESIAN_POINT('Ctrl Pts',(-2.00612458230317,6.2256306393371,-1.15823656762066));
#8345=CARTESIAN_POINT('Ctrl Pts',(-1.00306229115158,6.16729730600376,-1.73735485143099));
#8346=CARTESIAN_POINT('Ctrl Pts',(-1.41843070519206E-16,6.10896397267043,
-2.31647313524132));
#8347=CARTESIAN_POINT('Ctrl Pts',(1.00306229115158,6.05063063933711,-1.73735485143099));
#8348=CARTESIAN_POINT('Ctrl Pts',(2.00612458230317,5.99229730600376,-1.15823656762066));
#8349=CARTESIAN_POINT('Ctrl Pts',(2.00612458230317,5.93396397267044,-2.45679404840839E-16));
#8350=CARTESIAN_POINT('Ctrl Pts',(2.00612458230317,5.8756306393371,1.15823656762066));
#8351=CARTESIAN_POINT('Ctrl Pts',(1.00306229115158,5.81729730600377,1.73735485143099));
#8352=CARTESIAN_POINT('Ctrl Pts',(4.25529211557617E-16,5.75896397267043,
2.31647313524132));
#8353=CARTESIAN_POINT('Ctrl Pts',(-1.00306229115158,5.7006306393371,1.73735485143099));
#8354=CARTESIAN_POINT('Ctrl Pts',(-2.00612458230316,5.64229730600376,1.15823656762066));
#8355=CARTESIAN_POINT('Ctrl Pts',(-2.00612458230317,5.58396397267043,0.));
#8356=CARTESIAN_POINT('Ctrl Pts',(-2.00612458230317,5.52563063933709,-1.15823656762066));
#8357=CARTESIAN_POINT('Ctrl Pts',(-1.00306229115158,5.46729730600377,-1.73735485143099));
#8358=CARTESIAN_POINT('Ctrl Pts',(-1.41843070519206E-16,5.40896397267043,
-2.31647313524132));
#8359=CARTESIAN_POINT('Ctrl Pts',(1.00306229115158,5.3506306393371,-1.73735485143099));
#8360=CARTESIAN_POINT('Ctrl Pts',(2.00612458230317,5.29229730600377,-1.15823656762066));
#8361=CARTESIAN_POINT('Ctrl Pts',(2.00612458230317,5.23396397267043,-2.45679404840839E-16));
#8362=CARTESIAN_POINT('Ctrl Pts',(2.00612458230317,5.1756306393371,1.15823656762066));
#8363=CARTESIAN_POINT('Ctrl Pts',(1.00306229115158,5.11729730600376,1.73735485143099));
#8364=CARTESIAN_POINT('Ctrl Pts',(4.25529211557617E-16,5.05896397267044,
2.31647313524132));
#8365=CARTESIAN_POINT('Ctrl Pts',(-1.00306229115158,5.0006306393371,1.73735485143099));
#8366=CARTESIAN_POINT('Ctrl Pts',(-2.00612458230316,4.94229730600377,1.15823656762066));
#8367=CARTESIAN_POINT('Ctrl Pts',(-2.00612458230317,4.88396397267043,0.));
#8368=CARTESIAN_POINT('Ctrl Pts',(-2.00612458230317,4.8256306393371,-1.15823656762066));
#8369=CARTESIAN_POINT('Ctrl Pts',(-1.00306229115158,4.76729730600376,-1.73735485143099));
#8370=CARTESIAN_POINT('Ctrl Pts',(-1.41843070519206E-16,4.70896397267043,
-2.31647313524132));
#8371=CARTESIAN_POINT('Ctrl Pts',(1.00306229115158,4.65063063933709,-1.73735485143099));
#8372=CARTESIAN_POINT('Ctrl Pts',(2.00612458230317,4.59229730600377,-1.15823656762066));
#8373=CARTESIAN_POINT('Ctrl Pts',(2.00612458230317,4.53396397267044,-2.45679404840839E-16));
#8374=CARTESIAN_POINT('Ctrl Pts',(2.00612458230317,4.4756306393371,1.15823656762066));
#8375=CARTESIAN_POINT('Ctrl Pts',(1.00306229115158,4.41729730600377,1.73735485143099));
#8376=CARTESIAN_POINT('Ctrl Pts',(4.25529211557617E-16,4.35896397267043,
2.31647313524132));
#8377=CARTESIAN_POINT('Ctrl Pts',(-1.00306229115158,4.3006306393371,1.73735485143099));
#8378=CARTESIAN_POINT('Ctrl Pts',(-2.00612458230316,4.24229730600376,1.15823656762066));
#8379=CARTESIAN_POINT('Ctrl Pts',(-2.00612458230317,4.18396397267044,0.));
#8380=CARTESIAN_POINT('Ctrl Pts',(-2.00612458230317,4.1256306393371,-1.15823656762066));
#8381=CARTESIAN_POINT('Ctrl Pts',(-1.00306229115158,4.06729730600377,-1.73735485143099));
#8382=CARTESIAN_POINT('Ctrl Pts',(-1.41843070519206E-16,4.00896397267043,
-2.31647313524132));
#8383=CARTESIAN_POINT('Ctrl Pts',(1.00306229115158,3.9506306393371,-1.73735485143099));
#8384=CARTESIAN_POINT('Ctrl Pts',(2.00612458230317,3.89229730600376,-1.15823656762066));
#8385=CARTESIAN_POINT('Ctrl Pts',(2.00612458230317,3.83396397267043,-2.45679404840839E-16));
#8386=CARTESIAN_POINT('Ctrl Pts',(2.00612458230317,3.77563063933711,1.15823656762066));
#8387=CARTESIAN_POINT('Ctrl Pts',(1.00306229115158,3.71729730600377,1.73735485143099));
#8388=CARTESIAN_POINT('Ctrl Pts',(4.25529211557617E-16,3.65896397267044,
2.31647313524132));
#8389=CARTESIAN_POINT('Ctrl Pts',(-1.00306229115158,3.6006306393371,1.73735485143099));
#8390=CARTESIAN_POINT('Ctrl Pts',(-2.00612458230316,3.54229730600377,1.15823656762066));
#8391=CARTESIAN_POINT('Ctrl Pts',(-2.00612458230317,3.48396397267043,0.));
#8392=CARTESIAN_POINT('Ctrl Pts',(-2.00612458230317,3.4256306393371,-1.15823656762066));
#8393=CARTESIAN_POINT('Ctrl Pts',(-1.00306229115158,3.36729730600376,-1.73735485143099));
#8394=CARTESIAN_POINT('Ctrl Pts',(-1.41843070519206E-16,3.30896397267044,
-2.31647313524132));
#8395=CARTESIAN_POINT('Ctrl Pts',(1.00306229115158,3.25063063933709,-1.73735485143099));
#8396=CARTESIAN_POINT('Ctrl Pts',(2.00612458230317,3.19229730600377,-1.15823656762066));
#8397=CARTESIAN_POINT('Ctrl Pts',(2.00612458230317,3.13396397267043,-2.45679404840839E-16));
#8398=CARTESIAN_POINT('Ctrl Pts',(2.00612458230317,3.0756306393371,1.15823656762066));
#8399=CARTESIAN_POINT('Ctrl Pts',(1.00306229115158,3.01729730600376,1.73735485143099));
#8400=CARTESIAN_POINT('Ctrl Pts',(4.25529211557617E-16,2.95896397267043,
2.31647313524132));
#8401=CARTESIAN_POINT('Ctrl Pts',(-1.00306229115158,2.90063063933711,1.73735485143099));
#8402=CARTESIAN_POINT('Ctrl Pts',(-2.00612458230316,2.84229730600376,1.15823656762066));
#8403=CARTESIAN_POINT('Ctrl Pts',(-2.00612458230317,2.78396397267044,0.));
#8404=CARTESIAN_POINT('Ctrl Pts',(-2.00612458230317,2.7256306393371,-1.15823656762066));
#8405=CARTESIAN_POINT('Ctrl Pts',(-1.00306229115158,2.66729730600377,-1.73735485143099));
#8406=CARTESIAN_POINT('Ctrl Pts',(-1.41843070519206E-16,2.60896397267043,
-2.31647313524132));
#8407=CARTESIAN_POINT('Ctrl Pts',(1.00306229115158,2.5506306393371,-1.73735485143099));
#8408=CARTESIAN_POINT('Ctrl Pts',(2.00612458230317,2.49229730600376,-1.15823656762066));
#8409=CARTESIAN_POINT('Ctrl Pts',(2.00612458230317,2.43396397267043,-2.45679404840839E-16));
#8410=CARTESIAN_POINT('Ctrl Pts',(2.00612458230317,2.37563063933709,1.15823656762066));
#8411=CARTESIAN_POINT('Ctrl Pts',(1.00306229115158,2.31729730600377,1.73735485143099));
#8412=CARTESIAN_POINT('Ctrl Pts',(4.25529211557617E-16,2.25896397267043,
2.31647313524132));
#8413=CARTESIAN_POINT('Ctrl Pts',(-1.00306229115158,2.2006306393371,1.73735485143099));
#8414=CARTESIAN_POINT('Ctrl Pts',(-2.00612458230316,2.14229730600377,1.15823656762066));
#8415=CARTESIAN_POINT('Ctrl Pts',(-2.00612458230317,2.08396397267043,0.));
#8416=CARTESIAN_POINT('Ctrl Pts',(-2.00612458230317,2.0256306393371,-1.15823656762066));
#8417=CARTESIAN_POINT('Ctrl Pts',(-1.00306229115158,1.96729730600376,-1.73735485143099));
#8418=CARTESIAN_POINT('Ctrl Pts',(-1.41843070519206E-16,1.90896397267044,
-2.31647313524132));
#8419=CARTESIAN_POINT('Ctrl Pts',(1.00306229115158,1.8506306393371,-1.73735485143099));
#8420=CARTESIAN_POINT('Ctrl Pts',(2.00612458230317,1.79229730600377,-1.15823656762066));
#8421=CARTESIAN_POINT('Ctrl Pts',(2.00612458230317,1.73396397267043,-2.45679404840839E-16));
#8422=CARTESIAN_POINT('Ctrl Pts',(2.00612458230317,1.6756306393371,1.15823656762066));
#8423=CARTESIAN_POINT('Ctrl Pts',(1.00306229115158,1.61729730600376,1.73735485143099));
#8424=CARTESIAN_POINT('Ctrl Pts',(4.25529211557617E-16,1.55896397267043,
2.31647313524132));
#8425=CARTESIAN_POINT('Ctrl Pts',(-1.00306229115158,1.50063063933709,1.73735485143099));
#8426=CARTESIAN_POINT('Ctrl Pts',(-2.00612458230316,1.44229730600377,1.15823656762066));
#8427=CARTESIAN_POINT('Ctrl Pts',(-2.00612458230317,1.38396397267044,0.));
#8428=CARTESIAN_POINT('Ctrl Pts',(-2.00612458230317,1.3256306393371,-1.15823656762066));
#8429=CARTESIAN_POINT('Ctrl Pts',(-1.00306229115158,1.26729730600377,-1.73735485143099));
#8430=CARTESIAN_POINT('Ctrl Pts',(-1.41843070519206E-16,1.20896397267043,
-2.31647313524132));
#8431=CARTESIAN_POINT('Ctrl Pts',(1.00306229115158,1.1506306393371,-1.73735485143099));
#8432=CARTESIAN_POINT('Ctrl Pts',(2.00612458230317,1.09229730600376,-1.15823656762066));
#8433=CARTESIAN_POINT('Ctrl Pts',(2.00612458230317,1.03396397267044,-2.45679404840839E-16));
#8434=CARTESIAN_POINT('Ctrl Pts',(2.00612458230317,0.975630639337095,1.15823656762066));
#8435=CARTESIAN_POINT('Ctrl Pts',(1.00306229115158,0.917297306003768,1.73735485143099));
#8436=CARTESIAN_POINT('Ctrl Pts',(4.25529211557617E-16,0.858963972670427,
2.31647313524132));
#8437=CARTESIAN_POINT('Ctrl Pts',(-1.00306229115158,0.800630639337101,1.73735485143099));
#8438=CARTESIAN_POINT('Ctrl Pts',(-2.00612458230316,0.74229730600376,1.15823656762066));
#8439=CARTESIAN_POINT('Ctrl Pts',(-2.00612458230317,0.683963972670433,0.));
#8440=CARTESIAN_POINT('Ctrl Pts',(-2.00612458230317,0.625630639337106,-1.15823656762066));
#8441=CARTESIAN_POINT('Ctrl Pts',(-1.00306229115158,0.567297306003765,-1.73735485143099));
#8442=CARTESIAN_POINT('Ctrl Pts',(-1.41843070519206E-16,0.508963972670438,
-2.31647313524132));
#8443=CARTESIAN_POINT('Ctrl Pts',(1.00306229115158,0.450630639337097,-1.73735485143099));
#8444=CARTESIAN_POINT('Ctrl Pts',(2.00612458230317,0.39229730600377,-1.15823656762066));
#8445=CARTESIAN_POINT('Ctrl Pts',(2.00612458230317,0.33396397267043,-2.45679404840839E-16));
#8446=CARTESIAN_POINT('Ctrl Pts',(2.00612458230317,0.275630639337103,1.15823656762066));
#8447=CARTESIAN_POINT('Ctrl Pts',(1.00306229115158,0.217297306003762,1.73735485143099));
#8448=CARTESIAN_POINT('Ctrl Pts',(4.25529211557617E-16,0.158963972670435,
2.31647313524132));
#8449=CARTESIAN_POINT('Ctrl Pts',(-1.00306229115158,0.100630639337094,1.73735485143099));
#8450=CARTESIAN_POINT('Ctrl Pts',(-2.00612458230316,0.0422973060037674,
1.15823656762066));
#8451=CARTESIAN_POINT('Ctrl Pts',(-2.00612458230317,-0.0160360273295734,
0.));
#8452=CARTESIAN_POINT('Ctrl Pts',(-2.00612458230317,-0.0743693606629003,
-1.15823656762066));
#8453=CARTESIAN_POINT('Ctrl Pts',(-1.00306229115158,-0.132702693996241,
-1.73735485143099));
#8454=CARTESIAN_POINT('Ctrl Pts',(-1.41843070519206E-16,-0.191036027329568,
-2.31647313524132));
#8455=CARTESIAN_POINT('Ctrl Pts',(1.00306229115158,-0.249369360662895,-1.73735485143099));
#8456=CARTESIAN_POINT('Ctrl Pts',(2.00612458230317,-0.307702693996236,-1.15823656762066));
#8457=CARTESIAN_POINT('Ctrl Pts',(2.00612458230317,-0.366036027329563,-2.45679404840839E-16));
#8458=CARTESIAN_POINT('Ctrl Pts',(2.00612458230317,-0.424369360662903,1.15823656762066));
#8459=CARTESIAN_POINT('Ctrl Pts',(1.00306229115158,-0.48270269399623,1.73735485143099));
#8460=CARTESIAN_POINT('Ctrl Pts',(4.25529211557617E-16,-0.541036027329571,
2.31647313524132));
#8461=CARTESIAN_POINT('Ctrl Pts',(-1.00306229115158,-0.599369360662898,
1.73735485143099));
#8462=CARTESIAN_POINT('Ctrl Pts',(-2.00612458230316,-0.657702693996238,
1.15823656762066));
#8463=CARTESIAN_POINT('Ctrl Pts',(-2.00612458230317,-0.716036027329566,
0.));
#8464=CARTESIAN_POINT('Ctrl Pts',(-2.00612458230317,-0.774369360662906,
-1.15823656762066));
#8465=CARTESIAN_POINT('Ctrl Pts',(-1.00306229115158,-0.832702693996233,
-1.73735485143099));
#8466=CARTESIAN_POINT('Ctrl Pts',(-1.41843070519206E-16,-0.891036027329575,
-2.31647313524132));
#8467=CARTESIAN_POINT('Ctrl Pts',(1.00306229115158,-0.949369360662901,-1.73735485143099));
#8468=CARTESIAN_POINT('Ctrl Pts',(2.00612458230317,-1.00770269399623,-1.15823656762066));
#8469=CARTESIAN_POINT('Ctrl Pts',(2.00612458230317,-1.06603602732957,-2.45679404840839E-16));
#8470=CARTESIAN_POINT('Ctrl Pts',(2.00612458230317,-1.1243693606629,1.15823656762066));
#8471=CARTESIAN_POINT('Ctrl Pts',(1.00306229115158,-1.18270269399624,1.73735485143099));
#8472=CARTESIAN_POINT('Ctrl Pts',(4.25529211557617E-16,-1.24103602732956,
2.31647313524132));
#8473=CARTESIAN_POINT('Ctrl Pts',(-1.00306229115158,-1.2993693606629,1.73735485143099));
#8474=CARTESIAN_POINT('Ctrl Pts',(-2.00612458230316,-1.35770269399623,1.15823656762066));
#8475=CARTESIAN_POINT('Ctrl Pts',(-2.00612458230317,-1.41603602732957,0.));
#8476=CARTESIAN_POINT('Ctrl Pts',(-2.00612458230317,-1.4743693606629,-1.15823656762066));
#8477=CARTESIAN_POINT('Ctrl Pts',(-1.00306229115158,-1.53270269399624,-1.73735485143099));
#8478=CARTESIAN_POINT('Ctrl Pts',(-1.41843070519206E-16,-1.59103602732957,
-2.31647313524132));
#8479=CARTESIAN_POINT('Ctrl Pts',(1.00306229115158,-1.64936936066291,-1.73735485143099));
#8480=CARTESIAN_POINT('Ctrl Pts',(2.00612458230317,-1.70770269399623,-1.15823656762066));
#8481=CARTESIAN_POINT('Ctrl Pts',(2.00612458230317,-1.76603602732956,-2.45679404840839E-16));
#8482=CARTESIAN_POINT('Ctrl Pts',(2.00612458230317,-1.8243693606629,1.15823656762066));
#8483=CARTESIAN_POINT('Ctrl Pts',(1.00306229115158,-1.88270269399623,1.73735485143099));
#8484=CARTESIAN_POINT('Ctrl Pts',(4.25529211557617E-16,-1.94103602732957,
2.31647313524132));
#8485=CARTESIAN_POINT('Ctrl Pts',(-1.00306229115158,-1.9993693606629,1.73735485143099));
#8486=CARTESIAN_POINT('Ctrl Pts',(-2.00612458230316,-2.05770269399624,1.15823656762066));
#8487=CARTESIAN_POINT('Ctrl Pts',(-2.00612458230317,-2.11603602732956,0.));
#8488=CARTESIAN_POINT('Ctrl Pts',(-2.00612458230317,-2.17436936066291,-1.15823656762066));
#8489=CARTESIAN_POINT('Ctrl Pts',(-1.00306229115158,-2.23270269399623,-1.73735485143099));
#8490=CARTESIAN_POINT('Ctrl Pts',(-1.41843070519206E-16,-2.29103602732957,
-2.31647313524132));
#8491=CARTESIAN_POINT('Ctrl Pts',(1.00306229115158,-2.3493693606629,-1.73735485143099));
#8492=CARTESIAN_POINT('Ctrl Pts',(2.00612458230317,-2.40770269399624,-1.15823656762066));
#8493=CARTESIAN_POINT('Ctrl Pts',(2.00612458230317,-2.46603602732957,-2.45679404840839E-16));
#8494=CARTESIAN_POINT('Ctrl Pts',(2.00612458230317,-2.52436936066289,1.15823656762066));
#8495=CARTESIAN_POINT('Ctrl Pts',(1.00306229115158,-2.58270269399623,1.73735485143099));
#8496=CARTESIAN_POINT('Ctrl Pts',(0.74117398807312,-2.59793287243514,1.88855613371095));
#8497=CARTESIAN_POINT('Ctrl Pts',(0.446351454824861,-2.61507834909981,1.95583900628267));
#8498=CARTESIAN_POINT('Ctrl Pts',(-1.6211138875,71.6062500009559,0.));
#8499=CARTESIAN_POINT('Ctrl Pts',(-1.6211138875,71.5479166676226,-0.935950539335166));
#8500=CARTESIAN_POINT('Ctrl Pts',(-0.81055694375,71.4895833342893,-1.40392580900275));
#8501=CARTESIAN_POINT('Ctrl Pts',(-1.14620883215705E-16,71.4312500009559,
-1.87190107867033));
#8502=CARTESIAN_POINT('Ctrl Pts',(0.81055694375,71.3729166676226,-1.40392580900275));
#8503=CARTESIAN_POINT('Ctrl Pts',(1.6211138875,71.3145833342893,-0.935950539335166));
#8504=CARTESIAN_POINT('Ctrl Pts',(1.6211138875,71.2562500009559,-1.9852919333802E-16));
#8505=CARTESIAN_POINT('Ctrl Pts',(1.6211138875,71.1979166676226,0.935950539335165));
#8506=CARTESIAN_POINT('Ctrl Pts',(0.810556943750001,71.1395833342893,1.40392580900275));
#8507=CARTESIAN_POINT('Ctrl Pts',(3.43862649647115E-16,71.0812500009559,
1.87190107867033));
#8508=CARTESIAN_POINT('Ctrl Pts',(-0.810556943749999,71.0229166676226,1.40392580900275));
#8509=CARTESIAN_POINT('Ctrl Pts',(-1.6211138875,70.9645833342893,0.935950539335167));
#8510=CARTESIAN_POINT('Ctrl Pts',(-1.6211138875,70.9062500009559,0.));
#8511=CARTESIAN_POINT('Ctrl Pts',(-1.6211138875,70.8479166676226,-0.935950539335166));
#8512=CARTESIAN_POINT('Ctrl Pts',(-0.81055694375,70.7895833342893,-1.40392580900275));
#8513=CARTESIAN_POINT('Ctrl Pts',(-1.14620883215705E-16,70.7312500009559,
-1.87190107867033));
#8514=CARTESIAN_POINT('Ctrl Pts',(0.81055694375,70.6729166676226,-1.40392580900275));
#8515=CARTESIAN_POINT('Ctrl Pts',(1.6211138875,70.6145833342893,-0.935950539335166));
#8516=CARTESIAN_POINT('Ctrl Pts',(1.6211138875,70.5562500009559,-1.9852919333802E-16));
#8517=CARTESIAN_POINT('Ctrl Pts',(1.6211138875,70.4979166676226,0.935950539335165));
#8518=CARTESIAN_POINT('Ctrl Pts',(0.810556943750001,70.4395833342893,1.40392580900275));
#8519=CARTESIAN_POINT('Ctrl Pts',(3.43862649647115E-16,70.3812500009559,
1.87190107867033));
#8520=CARTESIAN_POINT('Ctrl Pts',(-0.810556943749999,70.3229166676226,1.40392580900275));
#8521=CARTESIAN_POINT('Ctrl Pts',(-1.6211138875,70.2645833342893,0.935950539335167));
#8522=CARTESIAN_POINT('Ctrl Pts',(-1.6211138875,70.2062500009559,0.));
#8523=CARTESIAN_POINT('Ctrl Pts',(-1.6211138875,70.1479166676226,-0.935950539335166));
#8524=CARTESIAN_POINT('Ctrl Pts',(-0.81055694375,70.0895833342893,-1.40392580900275));
#8525=CARTESIAN_POINT('Ctrl Pts',(-1.14620883215705E-16,70.0312500009559,
-1.87190107867033));
#8526=CARTESIAN_POINT('Ctrl Pts',(0.81055694375,69.9729166676226,-1.40392580900275));
#8527=CARTESIAN_POINT('Ctrl Pts',(1.6211138875,69.9145833342893,-0.935950539335166));
#8528=CARTESIAN_POINT('Ctrl Pts',(1.6211138875,69.8562500009559,-1.9852919333802E-16));
#8529=CARTESIAN_POINT('Ctrl Pts',(1.6211138875,69.7979166676226,0.935950539335165));
#8530=CARTESIAN_POINT('Ctrl Pts',(0.810556943750001,69.7395833342893,1.40392580900275));
#8531=CARTESIAN_POINT('Ctrl Pts',(3.43862649647115E-16,69.6812500009559,
1.87190107867033));
#8532=CARTESIAN_POINT('Ctrl Pts',(-0.810556943749999,69.6229166676226,1.40392580900275));
#8533=CARTESIAN_POINT('Ctrl Pts',(-1.6211138875,69.5645833342893,0.935950539335167));
#8534=CARTESIAN_POINT('Ctrl Pts',(-1.6211138875,69.5062500009559,0.));
#8535=CARTESIAN_POINT('Ctrl Pts',(-1.6211138875,69.4479166676226,-0.935950539335166));
#8536=CARTESIAN_POINT('Ctrl Pts',(-0.81055694375,69.3895833342893,-1.40392580900275));
#8537=CARTESIAN_POINT('Ctrl Pts',(-1.14620883215705E-16,69.3312500009559,
-1.87190107867033));
#8538=CARTESIAN_POINT('Ctrl Pts',(0.81055694375,69.2729166676226,-1.40392580900275));
#8539=CARTESIAN_POINT('Ctrl Pts',(1.6211138875,69.2145833342893,-0.935950539335166));
#8540=CARTESIAN_POINT('Ctrl Pts',(1.6211138875,69.1562500009559,-1.9852919333802E-16));
#8541=CARTESIAN_POINT('Ctrl Pts',(1.6211138875,69.0979166676226,0.935950539335165));
#8542=CARTESIAN_POINT('Ctrl Pts',(0.810556943750001,69.0395833342893,1.40392580900275));
#8543=CARTESIAN_POINT('Ctrl Pts',(3.43862649647115E-16,68.9812500009559,
1.87190107867033));
#8544=CARTESIAN_POINT('Ctrl Pts',(-0.810556943749999,68.9229166676226,1.40392580900275));
#8545=CARTESIAN_POINT('Ctrl Pts',(-1.6211138875,68.8645833342893,0.935950539335167));
#8546=CARTESIAN_POINT('Ctrl Pts',(-1.6211138875,68.8062500009559,0.));
#8547=CARTESIAN_POINT('Ctrl Pts',(-1.6211138875,68.7479166676226,-0.935950539335166));
#8548=CARTESIAN_POINT('Ctrl Pts',(-0.81055694375,68.6895833342893,-1.40392580900275));
#8549=CARTESIAN_POINT('Ctrl Pts',(-1.14620883215705E-16,68.6312500009559,
-1.87190107867033));
#8550=CARTESIAN_POINT('Ctrl Pts',(0.81055694375,68.5729166676226,-1.40392580900275));
#8551=CARTESIAN_POINT('Ctrl Pts',(1.6211138875,68.5145833342893,-0.935950539335166));
#8552=CARTESIAN_POINT('Ctrl Pts',(1.6211138875,68.4562500009559,-1.9852919333802E-16));
#8553=CARTESIAN_POINT('Ctrl Pts',(1.6211138875,68.3979166676226,0.935950539335165));
#8554=CARTESIAN_POINT('Ctrl Pts',(0.810556943750001,68.3395833342893,1.40392580900275));
#8555=CARTESIAN_POINT('Ctrl Pts',(3.43862649647115E-16,68.2812500009559,
1.87190107867033));
#8556=CARTESIAN_POINT('Ctrl Pts',(-0.810556943749999,68.2229166676226,1.40392580900275));
#8557=CARTESIAN_POINT('Ctrl Pts',(-1.6211138875,68.1645833342893,0.935950539335167));
#8558=CARTESIAN_POINT('Ctrl Pts',(-1.6211138875,68.1062500009559,0.));
#8559=CARTESIAN_POINT('Ctrl Pts',(-1.6211138875,68.0479166676226,-0.935950539335166));
#8560=CARTESIAN_POINT('Ctrl Pts',(-0.81055694375,67.9895833342893,-1.40392580900275));
#8561=CARTESIAN_POINT('Ctrl Pts',(-1.14620883215705E-16,67.9312500009559,
-1.87190107867033));
#8562=CARTESIAN_POINT('Ctrl Pts',(0.81055694375,67.8729166676226,-1.40392580900275));
#8563=CARTESIAN_POINT('Ctrl Pts',(1.6211138875,67.8145833342893,-0.935950539335166));
#8564=CARTESIAN_POINT('Ctrl Pts',(1.6211138875,67.7562500009559,-1.9852919333802E-16));
#8565=CARTESIAN_POINT('Ctrl Pts',(1.6211138875,67.6979166676226,0.935950539335165));
#8566=CARTESIAN_POINT('Ctrl Pts',(0.810556943750001,67.6395833342893,1.40392580900275));
#8567=CARTESIAN_POINT('Ctrl Pts',(3.43862649647115E-16,67.5812500009559,
1.87190107867033));
#8568=CARTESIAN_POINT('Ctrl Pts',(-0.810556943749999,67.5229166676226,1.40392580900275));
#8569=CARTESIAN_POINT('Ctrl Pts',(-1.6211138875,67.4645833342893,0.935950539335167));
#8570=CARTESIAN_POINT('Ctrl Pts',(-1.6211138875,67.4062500009559,0.));
#8571=CARTESIAN_POINT('Ctrl Pts',(-1.6211138875,67.3479166676226,-0.935950539335166));
#8572=CARTESIAN_POINT('Ctrl Pts',(-0.81055694375,67.2895833342893,-1.40392580900275));
#8573=CARTESIAN_POINT('Ctrl Pts',(-1.14620883215705E-16,67.2312500009559,
-1.87190107867033));
#8574=CARTESIAN_POINT('Ctrl Pts',(0.81055694375,67.1729166676226,-1.40392580900275));
#8575=CARTESIAN_POINT('Ctrl Pts',(1.6211138875,67.1145833342893,-0.935950539335166));
#8576=CARTESIAN_POINT('Ctrl Pts',(1.6211138875,67.0562500009559,-1.9852919333802E-16));
#8577=CARTESIAN_POINT('Ctrl Pts',(1.6211138875,66.9979166676226,0.935950539335165));
#8578=CARTESIAN_POINT('Ctrl Pts',(0.810556943750001,66.9395833342893,1.40392580900275));
#8579=CARTESIAN_POINT('Ctrl Pts',(3.43862649647115E-16,66.8812500009559,
1.87190107867033));
#8580=CARTESIAN_POINT('Ctrl Pts',(-0.810556943749999,66.8229166676226,1.40392580900275));
#8581=CARTESIAN_POINT('Ctrl Pts',(-1.6211138875,66.7645833342893,0.935950539335167));
#8582=CARTESIAN_POINT('Ctrl Pts',(-1.6211138875,66.7062500009559,0.));
#8583=CARTESIAN_POINT('Ctrl Pts',(-1.6211138875,66.6479166676226,-0.935950539335166));
#8584=CARTESIAN_POINT('Ctrl Pts',(-0.81055694375,66.5895833342893,-1.40392580900275));
#8585=CARTESIAN_POINT('Ctrl Pts',(-1.14620883215705E-16,66.5312500009559,
-1.87190107867033));
#8586=CARTESIAN_POINT('Ctrl Pts',(0.81055694375,66.4729166676226,-1.40392580900275));
#8587=CARTESIAN_POINT('Ctrl Pts',(1.6211138875,66.4145833342893,-0.935950539335166));
#8588=CARTESIAN_POINT('Ctrl Pts',(1.6211138875,66.3562500009559,-1.9852919333802E-16));
#8589=CARTESIAN_POINT('Ctrl Pts',(1.6211138875,66.2979166676226,0.935950539335165));
#8590=CARTESIAN_POINT('Ctrl Pts',(0.810556943750001,66.2395833342893,1.40392580900275));
#8591=CARTESIAN_POINT('Ctrl Pts',(3.43862649647115E-16,66.1812500009559,
1.87190107867033));
#8592=CARTESIAN_POINT('Ctrl Pts',(-0.810556943749999,66.1229166676226,1.40392580900275));
#8593=CARTESIAN_POINT('Ctrl Pts',(-1.6211138875,66.0645833342893,0.935950539335167));
#8594=CARTESIAN_POINT('Ctrl Pts',(-1.6211138875,66.0062500009559,0.));
#8595=CARTESIAN_POINT('Ctrl Pts',(-1.6211138875,65.9479166676226,-0.935950539335166));
#8596=CARTESIAN_POINT('Ctrl Pts',(-0.81055694375,65.8895833342893,-1.40392580900275));
#8597=CARTESIAN_POINT('Ctrl Pts',(-1.14620883215705E-16,65.8312500009559,
-1.87190107867033));
#8598=CARTESIAN_POINT('Ctrl Pts',(0.81055694375,65.7729166676226,-1.40392580900275));
#8599=CARTESIAN_POINT('Ctrl Pts',(1.6211138875,65.7145833342893,-0.935950539335166));
#8600=CARTESIAN_POINT('Ctrl Pts',(1.6211138875,65.6562500009559,-1.9852919333802E-16));
#8601=CARTESIAN_POINT('Ctrl Pts',(1.6211138875,65.5979166676226,0.935950539335165));
#8602=CARTESIAN_POINT('Ctrl Pts',(0.810556943750001,65.5395833342893,1.40392580900275));
#8603=CARTESIAN_POINT('Ctrl Pts',(3.43862649647115E-16,65.4812500009559,
1.87190107867033));
#8604=CARTESIAN_POINT('Ctrl Pts',(-0.810556943749999,65.4229166676226,1.40392580900275));
#8605=CARTESIAN_POINT('Ctrl Pts',(-1.6211138875,65.3645833342893,0.935950539335167));
#8606=CARTESIAN_POINT('Ctrl Pts',(-1.6211138875,65.3062500009559,0.));
#8607=CARTESIAN_POINT('Ctrl Pts',(-1.6211138875,65.2479166676226,-0.935950539335166));
#8608=CARTESIAN_POINT('Ctrl Pts',(-0.81055694375,65.1895833342893,-1.40392580900275));
#8609=CARTESIAN_POINT('Ctrl Pts',(-1.14620883215705E-16,65.1312500009559,
-1.87190107867033));
#8610=CARTESIAN_POINT('Ctrl Pts',(0.81055694375,65.0729166676226,-1.40392580900275));
#8611=CARTESIAN_POINT('Ctrl Pts',(1.6211138875,65.0145833342893,-0.935950539335166));
#8612=CARTESIAN_POINT('Ctrl Pts',(1.6211138875,64.9562500009559,-1.9852919333802E-16));
#8613=CARTESIAN_POINT('Ctrl Pts',(1.6211138875,64.8979166676226,0.935950539335165));
#8614=CARTESIAN_POINT('Ctrl Pts',(0.810556943750001,64.8395833342893,1.40392580900275));
#8615=CARTESIAN_POINT('Ctrl Pts',(3.43862649647115E-16,64.7812500009559,
1.87190107867033));
#8616=CARTESIAN_POINT('Ctrl Pts',(-0.810556943749999,64.7229166676226,1.40392580900275));
#8617=CARTESIAN_POINT('Ctrl Pts',(-1.6211138875,64.6645833342893,0.935950539335167));
#8618=CARTESIAN_POINT('Ctrl Pts',(-1.6211138875,64.6062500009559,0.));
#8619=CARTESIAN_POINT('Ctrl Pts',(-1.6211138875,64.5479166676226,-0.935950539335166));
#8620=CARTESIAN_POINT('Ctrl Pts',(-0.81055694375,64.4895833342893,-1.40392580900275));
#8621=CARTESIAN_POINT('Ctrl Pts',(-1.14620883215705E-16,64.4312500009559,
-1.87190107867033));
#8622=CARTESIAN_POINT('Ctrl Pts',(0.81055694375,64.3729166676226,-1.40392580900275));
#8623=CARTESIAN_POINT('Ctrl Pts',(1.6211138875,64.3145833342893,-0.935950539335166));
#8624=CARTESIAN_POINT('Ctrl Pts',(1.6211138875,64.2562500009559,-1.9852919333802E-16));
#8625=CARTESIAN_POINT('Ctrl Pts',(1.6211138875,64.1979166676226,0.935950539335165));
#8626=CARTESIAN_POINT('Ctrl Pts',(0.810556943750001,64.1395833342893,1.40392580900275));
#8627=CARTESIAN_POINT('Ctrl Pts',(3.43862649647115E-16,64.0812500009559,
1.87190107867033));
#8628=CARTESIAN_POINT('Ctrl Pts',(-0.810556943749999,64.0229166676226,1.40392580900275));
#8629=CARTESIAN_POINT('Ctrl Pts',(-1.6211138875,63.9645833342893,0.935950539335167));
#8630=CARTESIAN_POINT('Ctrl Pts',(-1.6211138875,63.9062500009559,0.));
#8631=CARTESIAN_POINT('Ctrl Pts',(-1.6211138875,63.8479166676226,-0.935950539335166));
#8632=CARTESIAN_POINT('Ctrl Pts',(-0.81055694375,63.7895833342893,-1.40392580900275));
#8633=CARTESIAN_POINT('Ctrl Pts',(-1.14620883215705E-16,63.7312500009559,
-1.87190107867033));
#8634=CARTESIAN_POINT('Ctrl Pts',(0.81055694375,63.6729166676226,-1.40392580900275));
#8635=CARTESIAN_POINT('Ctrl Pts',(1.6211138875,63.6145833342893,-0.935950539335166));
#8636=CARTESIAN_POINT('Ctrl Pts',(1.6211138875,63.5562500009559,-1.9852919333802E-16));
#8637=CARTESIAN_POINT('Ctrl Pts',(1.6211138875,63.4979166676226,0.935950539335165));
#8638=CARTESIAN_POINT('Ctrl Pts',(0.810556943750001,63.4395833342893,1.40392580900275));
#8639=CARTESIAN_POINT('Ctrl Pts',(3.43862649647115E-16,63.3812500009559,
1.87190107867033));
#8640=CARTESIAN_POINT('Ctrl Pts',(-0.810556943749999,63.3229166676226,1.40392580900275));
#8641=CARTESIAN_POINT('Ctrl Pts',(-1.6211138875,63.2645833342893,0.935950539335167));
#8642=CARTESIAN_POINT('Ctrl Pts',(-1.6211138875,63.2062500009559,0.));
#8643=CARTESIAN_POINT('Ctrl Pts',(-1.6211138875,63.1479166676226,-0.935950539335166));
#8644=CARTESIAN_POINT('Ctrl Pts',(-0.81055694375,63.0895833342893,-1.40392580900275));
#8645=CARTESIAN_POINT('Ctrl Pts',(-1.14620883215705E-16,63.0312500009559,
-1.87190107867033));
#8646=CARTESIAN_POINT('Ctrl Pts',(0.81055694375,62.9729166676226,-1.40392580900275));
#8647=CARTESIAN_POINT('Ctrl Pts',(1.6211138875,62.9145833342892,-0.935950539335166));
#8648=CARTESIAN_POINT('Ctrl Pts',(1.6211138875,62.8562500009559,-1.9852919333802E-16));
#8649=CARTESIAN_POINT('Ctrl Pts',(1.6211138875,62.7979166676226,0.935950539335165));
#8650=CARTESIAN_POINT('Ctrl Pts',(0.810556943750001,62.7395833342893,1.40392580900275));
#8651=CARTESIAN_POINT('Ctrl Pts',(3.43862649647115E-16,62.6812500009559,
1.87190107867033));
#8652=CARTESIAN_POINT('Ctrl Pts',(-0.810556943749999,62.6229166676226,1.40392580900275));
#8653=CARTESIAN_POINT('Ctrl Pts',(-1.6211138875,62.5645833342893,0.935950539335167));
#8654=CARTESIAN_POINT('Ctrl Pts',(-1.6211138875,62.5062500009559,0.));
#8655=CARTESIAN_POINT('Ctrl Pts',(-1.6211138875,62.4479166676226,-0.935950539335166));
#8656=CARTESIAN_POINT('Ctrl Pts',(-0.81055694375,62.3895833342893,-1.40392580900275));
#8657=CARTESIAN_POINT('Ctrl Pts',(-1.14620883215705E-16,62.3312500009559,
-1.87190107867033));
#8658=CARTESIAN_POINT('Ctrl Pts',(0.81055694375,62.2729166676226,-1.40392580900275));
#8659=CARTESIAN_POINT('Ctrl Pts',(1.6211138875,62.2145833342893,-0.935950539335166));
#8660=CARTESIAN_POINT('Ctrl Pts',(1.6211138875,62.1562500009559,-1.9852919333802E-16));
#8661=CARTESIAN_POINT('Ctrl Pts',(1.6211138875,62.0979166676226,0.935950539335165));
#8662=CARTESIAN_POINT('Ctrl Pts',(0.810556943750001,62.0395833342893,1.40392580900275));
#8663=CARTESIAN_POINT('Ctrl Pts',(3.43862649647115E-16,61.9812500009559,
1.87190107867033));
#8664=CARTESIAN_POINT('Ctrl Pts',(-0.810556943749999,61.9229166676226,1.40392580900275));
#8665=CARTESIAN_POINT('Ctrl Pts',(-1.6211138875,61.8645833342893,0.935950539335167));
#8666=CARTESIAN_POINT('Ctrl Pts',(-1.6211138875,61.8062500009559,0.));
#8667=CARTESIAN_POINT('Ctrl Pts',(-1.6211138875,61.7479166676226,-0.935950539335166));
#8668=CARTESIAN_POINT('Ctrl Pts',(-0.81055694375,61.6895833342893,-1.40392580900275));
#8669=CARTESIAN_POINT('Ctrl Pts',(-1.14620883215705E-16,61.6312500009559,
-1.87190107867033));
#8670=CARTESIAN_POINT('Ctrl Pts',(0.81055694375,61.5729166676226,-1.40392580900275));
#8671=CARTESIAN_POINT('Ctrl Pts',(1.6211138875,61.5145833342893,-0.935950539335166));
#8672=CARTESIAN_POINT('Ctrl Pts',(1.6211138875,61.4562500009559,-1.9852919333802E-16));
#8673=CARTESIAN_POINT('Ctrl Pts',(1.6211138875,61.3979166676226,0.935950539335165));
#8674=CARTESIAN_POINT('Ctrl Pts',(0.810556943750001,61.3395833342893,1.40392580900275));
#8675=CARTESIAN_POINT('Ctrl Pts',(3.43862649647115E-16,61.2812500009559,
1.87190107867033));
#8676=CARTESIAN_POINT('Ctrl Pts',(-0.810556943749999,61.2229166676226,1.40392580900275));
#8677=CARTESIAN_POINT('Ctrl Pts',(-1.6211138875,61.1645833342893,0.935950539335167));
#8678=CARTESIAN_POINT('Ctrl Pts',(-1.6211138875,61.1062500009559,0.));
#8679=CARTESIAN_POINT('Ctrl Pts',(-1.6211138875,61.0479166676226,-0.935950539335166));
#8680=CARTESIAN_POINT('Ctrl Pts',(-0.81055694375,60.9895833342893,-1.40392580900275));
#8681=CARTESIAN_POINT('Ctrl Pts',(-1.14620883215705E-16,60.9312500009559,
-1.87190107867033));
#8682=CARTESIAN_POINT('Ctrl Pts',(0.81055694375,60.8729166676226,-1.40392580900275));
#8683=CARTESIAN_POINT('Ctrl Pts',(1.6211138875,60.8145833342893,-0.935950539335166));
#8684=CARTESIAN_POINT('Ctrl Pts',(1.6211138875,60.7562500009559,-1.9852919333802E-16));
#8685=CARTESIAN_POINT('Ctrl Pts',(1.6211138875,60.6979166676226,0.935950539335165));
#8686=CARTESIAN_POINT('Ctrl Pts',(0.810556943750001,60.6395833342893,1.40392580900275));
#8687=CARTESIAN_POINT('Ctrl Pts',(3.43862649647115E-16,60.5812500009559,
1.87190107867033));
#8688=CARTESIAN_POINT('Ctrl Pts',(-0.810556943749999,60.5229166676226,1.40392580900275));
#8689=CARTESIAN_POINT('Ctrl Pts',(-1.6211138875,60.4645833342893,0.935950539335167));
#8690=CARTESIAN_POINT('Ctrl Pts',(-1.6211138875,60.4062500009559,0.));
#8691=CARTESIAN_POINT('Ctrl Pts',(-1.6211138875,60.3479166676226,-0.935950539335166));
#8692=CARTESIAN_POINT('Ctrl Pts',(-0.81055694375,60.2895833342893,-1.40392580900275));
#8693=CARTESIAN_POINT('Ctrl Pts',(-1.14620883215705E-16,60.2312500009559,
-1.87190107867033));
#8694=CARTESIAN_POINT('Ctrl Pts',(0.81055694375,60.1729166676226,-1.40392580900275));
#8695=CARTESIAN_POINT('Ctrl Pts',(1.6211138875,60.1145833342893,-0.935950539335166));
#8696=CARTESIAN_POINT('Ctrl Pts',(1.6211138875,60.0562500009559,-1.9852919333802E-16));
#8697=CARTESIAN_POINT('Ctrl Pts',(1.6211138875,59.9979166676226,0.935950539335165));
#8698=CARTESIAN_POINT('Ctrl Pts',(0.810556943750001,59.9395833342893,1.40392580900275));
#8699=CARTESIAN_POINT('Ctrl Pts',(3.43862649647115E-16,59.8812500009559,
1.87190107867033));
#8700=CARTESIAN_POINT('Ctrl Pts',(-0.810556943749999,59.8229166676226,1.40392580900275));
#8701=CARTESIAN_POINT('Ctrl Pts',(-1.6211138875,59.7645833342893,0.935950539335167));
#8702=CARTESIAN_POINT('Ctrl Pts',(-1.6211138875,59.7062500009559,0.));
#8703=CARTESIAN_POINT('Ctrl Pts',(-1.6211138875,59.6479166676226,-0.935950539335166));
#8704=CARTESIAN_POINT('Ctrl Pts',(-0.81055694375,59.5895833342893,-1.40392580900275));
#8705=CARTESIAN_POINT('Ctrl Pts',(-1.14620883215705E-16,59.5312500009559,
-1.87190107867033));
#8706=CARTESIAN_POINT('Ctrl Pts',(0.81055694375,59.4729166676226,-1.40392580900275));
#8707=CARTESIAN_POINT('Ctrl Pts',(1.6211138875,59.4145833342893,-0.935950539335166));
#8708=CARTESIAN_POINT('Ctrl Pts',(1.6211138875,59.3562500009559,-1.9852919333802E-16));
#8709=CARTESIAN_POINT('Ctrl Pts',(1.6211138875,59.2979166676226,0.935950539335165));
#8710=CARTESIAN_POINT('Ctrl Pts',(0.810556943750001,59.2395833342893,1.40392580900275));
#8711=CARTESIAN_POINT('Ctrl Pts',(3.43862649647115E-16,59.1812500009559,
1.87190107867033));
#8712=CARTESIAN_POINT('Ctrl Pts',(-0.810556943749999,59.1229166676226,1.40392580900275));
#8713=CARTESIAN_POINT('Ctrl Pts',(-1.6211138875,59.0645833342893,0.935950539335167));
#8714=CARTESIAN_POINT('Ctrl Pts',(-1.6211138875,59.0062500009559,0.));
#8715=CARTESIAN_POINT('Ctrl Pts',(-1.6211138875,58.9479166676226,-0.935950539335166));
#8716=CARTESIAN_POINT('Ctrl Pts',(-0.81055694375,58.8895833342893,-1.40392580900275));
#8717=CARTESIAN_POINT('Ctrl Pts',(-1.14620883215705E-16,58.8312500009559,
-1.87190107867033));
#8718=CARTESIAN_POINT('Ctrl Pts',(0.81055694375,58.7729166676226,-1.40392580900275));
#8719=CARTESIAN_POINT('Ctrl Pts',(1.6211138875,58.7145833342893,-0.935950539335166));
#8720=CARTESIAN_POINT('Ctrl Pts',(1.6211138875,58.6562500009559,-1.9852919333802E-16));
#8721=CARTESIAN_POINT('Ctrl Pts',(1.6211138875,58.5979166676226,0.935950539335165));
#8722=CARTESIAN_POINT('Ctrl Pts',(0.810556943750001,58.5395833342893,1.40392580900275));
#8723=CARTESIAN_POINT('Ctrl Pts',(3.43862649647115E-16,58.4812500009559,
1.87190107867033));
#8724=CARTESIAN_POINT('Ctrl Pts',(-0.810556943749999,58.4229166676226,1.40392580900275));
#8725=CARTESIAN_POINT('Ctrl Pts',(-1.6211138875,58.3645833342893,0.935950539335167));
#8726=CARTESIAN_POINT('Ctrl Pts',(-1.6211138875,58.3062500009559,0.));
#8727=CARTESIAN_POINT('Ctrl Pts',(-1.6211138875,58.2479166676226,-0.935950539335166));
#8728=CARTESIAN_POINT('Ctrl Pts',(-0.81055694375,58.1895833342893,-1.40392580900275));
#8729=CARTESIAN_POINT('Ctrl Pts',(-1.14620883215705E-16,58.1312500009559,
-1.87190107867033));
#8730=CARTESIAN_POINT('Ctrl Pts',(0.81055694375,58.0729166676226,-1.40392580900275));
#8731=CARTESIAN_POINT('Ctrl Pts',(1.6211138875,58.0145833342893,-0.935950539335166));
#8732=CARTESIAN_POINT('Ctrl Pts',(1.6211138875,57.9562500009559,-1.9852919333802E-16));
#8733=CARTESIAN_POINT('Ctrl Pts',(1.6211138875,57.8979166676226,0.935950539335165));
#8734=CARTESIAN_POINT('Ctrl Pts',(0.810556943750001,57.8395833342893,1.40392580900275));
#8735=CARTESIAN_POINT('Ctrl Pts',(3.43862649647115E-16,57.7812500009559,
1.87190107867033));
#8736=CARTESIAN_POINT('Ctrl Pts',(-0.810556943749999,57.7229166676226,1.40392580900275));
#8737=CARTESIAN_POINT('Ctrl Pts',(-1.6211138875,57.6645833342893,0.935950539335167));
#8738=CARTESIAN_POINT('Ctrl Pts',(-1.6211138875,57.6062500009559,0.));
#8739=CARTESIAN_POINT('Ctrl Pts',(-1.6211138875,57.5479166676226,-0.935950539335166));
#8740=CARTESIAN_POINT('Ctrl Pts',(-0.81055694375,57.4895833342893,-1.40392580900275));
#8741=CARTESIAN_POINT('Ctrl Pts',(-1.14620883215705E-16,57.4312500009559,
-1.87190107867033));
#8742=CARTESIAN_POINT('Ctrl Pts',(0.81055694375,57.3729166676226,-1.40392580900275));
#8743=CARTESIAN_POINT('Ctrl Pts',(1.6211138875,57.3145833342893,-0.935950539335166));
#8744=CARTESIAN_POINT('Ctrl Pts',(1.6211138875,57.2562500009559,-1.9852919333802E-16));
#8745=CARTESIAN_POINT('Ctrl Pts',(1.6211138875,57.1979166676226,0.935950539335165));
#8746=CARTESIAN_POINT('Ctrl Pts',(0.810556943750001,57.1395833342893,1.40392580900275));
#8747=CARTESIAN_POINT('Ctrl Pts',(3.43862649647115E-16,57.0812500009559,
1.87190107867033));
#8748=CARTESIAN_POINT('Ctrl Pts',(-0.810556943749999,57.0229166676226,1.40392580900275));
#8749=CARTESIAN_POINT('Ctrl Pts',(-1.6211138875,56.9645833342893,0.935950539335167));
#8750=CARTESIAN_POINT('Ctrl Pts',(-1.6211138875,56.9062500009559,0.));
#8751=CARTESIAN_POINT('Ctrl Pts',(-1.6211138875,56.8479166676226,-0.935950539335166));
#8752=CARTESIAN_POINT('Ctrl Pts',(-0.81055694375,56.7895833342893,-1.40392580900275));
#8753=CARTESIAN_POINT('Ctrl Pts',(-1.14620883215705E-16,56.7312500009559,
-1.87190107867033));
#8754=CARTESIAN_POINT('Ctrl Pts',(0.81055694375,56.6729166676226,-1.40392580900275));
#8755=CARTESIAN_POINT('Ctrl Pts',(1.6211138875,56.6145833342893,-0.935950539335166));
#8756=CARTESIAN_POINT('Ctrl Pts',(1.6211138875,56.5562500009559,-1.9852919333802E-16));
#8757=CARTESIAN_POINT('Ctrl Pts',(1.6211138875,56.4979166676226,0.935950539335165));
#8758=CARTESIAN_POINT('Ctrl Pts',(0.810556943750001,56.4395833342893,1.40392580900275));
#8759=CARTESIAN_POINT('Ctrl Pts',(3.43862649647115E-16,56.3812500009559,
1.87190107867033));
#8760=CARTESIAN_POINT('Ctrl Pts',(-0.810556943749999,56.3229166676226,1.40392580900275));
#8761=CARTESIAN_POINT('Ctrl Pts',(-1.6211138875,56.2645833342893,0.935950539335167));
#8762=CARTESIAN_POINT('Ctrl Pts',(-1.6211138875,56.2062500009559,0.));
#8763=CARTESIAN_POINT('Ctrl Pts',(-1.6211138875,56.1479166676226,-0.935950539335166));
#8764=CARTESIAN_POINT('Ctrl Pts',(-0.81055694375,56.0895833342893,-1.40392580900275));
#8765=CARTESIAN_POINT('Ctrl Pts',(-1.14620883215705E-16,56.0312500009559,
-1.87190107867033));
#8766=CARTESIAN_POINT('Ctrl Pts',(0.81055694375,55.9729166676226,-1.40392580900275));
#8767=CARTESIAN_POINT('Ctrl Pts',(1.6211138875,55.9145833342893,-0.935950539335166));
#8768=CARTESIAN_POINT('Ctrl Pts',(1.6211138875,55.8562500009559,-1.9852919333802E-16));
#8769=CARTESIAN_POINT('Ctrl Pts',(1.6211138875,55.7979166676226,0.935950539335165));
#8770=CARTESIAN_POINT('Ctrl Pts',(0.810556943750001,55.7395833342893,1.40392580900275));
#8771=CARTESIAN_POINT('Ctrl Pts',(3.43862649647115E-16,55.6812500009559,
1.87190107867033));
#8772=CARTESIAN_POINT('Ctrl Pts',(-0.810556943749999,55.6229166676226,1.40392580900275));
#8773=CARTESIAN_POINT('Ctrl Pts',(-1.6211138875,55.5645833342893,0.935950539335167));
#8774=CARTESIAN_POINT('Ctrl Pts',(-1.6211138875,55.5062500009559,0.));
#8775=CARTESIAN_POINT('Ctrl Pts',(-1.6211138875,55.4479166676226,-0.935950539335166));
#8776=CARTESIAN_POINT('Ctrl Pts',(-0.81055694375,55.3895833342893,-1.40392580900275));
#8777=CARTESIAN_POINT('Ctrl Pts',(-1.14620883215705E-16,55.3312500009559,
-1.87190107867033));
#8778=CARTESIAN_POINT('Ctrl Pts',(0.81055694375,55.2729166676226,-1.40392580900275));
#8779=CARTESIAN_POINT('Ctrl Pts',(1.6211138875,55.2145833342893,-0.935950539335166));
#8780=CARTESIAN_POINT('Ctrl Pts',(1.6211138875,55.1562500009559,-1.9852919333802E-16));
#8781=CARTESIAN_POINT('Ctrl Pts',(1.6211138875,55.0979166676226,0.935950539335165));
#8782=CARTESIAN_POINT('Ctrl Pts',(0.810556943750001,55.0395833342893,1.40392580900275));
#8783=CARTESIAN_POINT('Ctrl Pts',(3.43862649647115E-16,54.9812500009559,
1.87190107867033));
#8784=CARTESIAN_POINT('Ctrl Pts',(-0.810556943749999,54.9229166676226,1.40392580900275));
#8785=CARTESIAN_POINT('Ctrl Pts',(-1.6211138875,54.8645833342893,0.935950539335167));
#8786=CARTESIAN_POINT('Ctrl Pts',(-1.6211138875,54.8062500009559,0.));
#8787=CARTESIAN_POINT('Ctrl Pts',(-1.6211138875,54.7479166676226,-0.935950539335166));
#8788=CARTESIAN_POINT('Ctrl Pts',(-0.81055694375,54.6895833342893,-1.40392580900275));
#8789=CARTESIAN_POINT('Ctrl Pts',(-1.14620883215705E-16,54.6312500009559,
-1.87190107867033));
#8790=CARTESIAN_POINT('Ctrl Pts',(0.81055694375,54.5729166676226,-1.40392580900275));
#8791=CARTESIAN_POINT('Ctrl Pts',(1.6211138875,54.5145833342892,-0.935950539335166));
#8792=CARTESIAN_POINT('Ctrl Pts',(1.6211138875,54.4562500009559,-1.9852919333802E-16));
#8793=CARTESIAN_POINT('Ctrl Pts',(1.6211138875,54.3979166676226,0.935950539335165));
#8794=CARTESIAN_POINT('Ctrl Pts',(0.810556943750001,54.3395833342893,1.40392580900275));
#8795=CARTESIAN_POINT('Ctrl Pts',(3.43862649647115E-16,54.2812500009559,
1.87190107867033));
#8796=CARTESIAN_POINT('Ctrl Pts',(-0.810556943749999,54.2229166676226,1.40392580900275));
#8797=CARTESIAN_POINT('Ctrl Pts',(-1.6211138875,54.1645833342893,0.935950539335167));
#8798=CARTESIAN_POINT('Ctrl Pts',(-1.6211138875,54.1062500009559,0.));
#8799=CARTESIAN_POINT('Ctrl Pts',(-1.6211138875,54.0479166676226,-0.935950539335166));
#8800=CARTESIAN_POINT('Ctrl Pts',(-0.81055694375,53.9895833342893,-1.40392580900275));
#8801=CARTESIAN_POINT('Ctrl Pts',(-1.14620883215705E-16,53.9312500009559,
-1.87190107867033));
#8802=CARTESIAN_POINT('Ctrl Pts',(0.81055694375,53.8729166676226,-1.40392580900275));
#8803=CARTESIAN_POINT('Ctrl Pts',(1.6211138875,53.8145833342893,-0.935950539335166));
#8804=CARTESIAN_POINT('Ctrl Pts',(1.6211138875,53.7562500009559,-1.9852919333802E-16));
#8805=CARTESIAN_POINT('Ctrl Pts',(1.6211138875,53.6979166676226,0.935950539335165));
#8806=CARTESIAN_POINT('Ctrl Pts',(0.810556943750001,53.6395833342893,1.40392580900275));
#8807=CARTESIAN_POINT('Ctrl Pts',(3.43862649647115E-16,53.5812500009559,
1.87190107867033));
#8808=CARTESIAN_POINT('Ctrl Pts',(-0.810556943749999,53.5229166676226,1.40392580900275));
#8809=CARTESIAN_POINT('Ctrl Pts',(-1.6211138875,53.4645833342893,0.935950539335167));
#8810=CARTESIAN_POINT('Ctrl Pts',(-1.6211138875,53.4062500009559,0.));
#8811=CARTESIAN_POINT('Ctrl Pts',(-1.6211138875,53.3479166676226,-0.935950539335166));
#8812=CARTESIAN_POINT('Ctrl Pts',(-0.81055694375,53.2895833342893,-1.40392580900275));
#8813=CARTESIAN_POINT('Ctrl Pts',(-1.14620883215705E-16,53.2312500009559,
-1.87190107867033));
#8814=CARTESIAN_POINT('Ctrl Pts',(0.81055694375,53.1729166676226,-1.40392580900275));
#8815=CARTESIAN_POINT('Ctrl Pts',(1.6211138875,53.1145833342893,-0.935950539335166));
#8816=CARTESIAN_POINT('Ctrl Pts',(1.6211138875,53.0562500009559,-1.9852919333802E-16));
#8817=CARTESIAN_POINT('Ctrl Pts',(1.6211138875,52.9979166676226,0.935950539335165));
#8818=CARTESIAN_POINT('Ctrl Pts',(0.810556943750001,52.9395833342893,1.40392580900275));
#8819=CARTESIAN_POINT('Ctrl Pts',(3.43862649647115E-16,52.8812500009559,
1.87190107867033));
#8820=CARTESIAN_POINT('Ctrl Pts',(-0.810556943749999,52.8229166676226,1.40392580900275));
#8821=CARTESIAN_POINT('Ctrl Pts',(-1.6211138875,52.7645833342893,0.935950539335167));
#8822=CARTESIAN_POINT('Ctrl Pts',(-1.6211138875,52.7062500009559,0.));
#8823=CARTESIAN_POINT('Ctrl Pts',(-1.6211138875,52.6479166676226,-0.935950539335166));
#8824=CARTESIAN_POINT('Ctrl Pts',(-0.81055694375,52.5895833342893,-1.40392580900275));
#8825=CARTESIAN_POINT('Ctrl Pts',(-1.14620883215705E-16,52.5312500009559,
-1.87190107867033));
#8826=CARTESIAN_POINT('Ctrl Pts',(0.81055694375,52.4729166676226,-1.40392580900275));
#8827=CARTESIAN_POINT('Ctrl Pts',(1.6211138875,52.4145833342893,-0.935950539335166));
#8828=CARTESIAN_POINT('Ctrl Pts',(1.6211138875,52.3562500009559,-1.9852919333802E-16));
#8829=CARTESIAN_POINT('Ctrl Pts',(1.6211138875,52.2979166676226,0.935950539335165));
#8830=CARTESIAN_POINT('Ctrl Pts',(0.810556943750001,52.2395833342893,1.40392580900275));
#8831=CARTESIAN_POINT('Ctrl Pts',(3.43862649647115E-16,52.1812500009559,
1.87190107867033));
#8832=CARTESIAN_POINT('Ctrl Pts',(-0.810556943749999,52.1229166676226,1.40392580900275));
#8833=CARTESIAN_POINT('Ctrl Pts',(-1.6211138875,52.0645833342893,0.935950539335167));
#8834=CARTESIAN_POINT('Ctrl Pts',(-1.6211138875,52.0062500009559,0.));
#8835=CARTESIAN_POINT('Ctrl Pts',(-1.6211138875,51.9479166676226,-0.935950539335166));
#8836=CARTESIAN_POINT('Ctrl Pts',(-0.81055694375,51.8895833342893,-1.40392580900275));
#8837=CARTESIAN_POINT('Ctrl Pts',(-1.14620883215705E-16,51.8312500009559,
-1.87190107867033));
#8838=CARTESIAN_POINT('Ctrl Pts',(0.81055694375,51.7729166676226,-1.40392580900275));
#8839=CARTESIAN_POINT('Ctrl Pts',(1.6211138875,51.7145833342893,-0.935950539335166));
#8840=CARTESIAN_POINT('Ctrl Pts',(1.6211138875,51.6562500009559,-1.9852919333802E-16));
#8841=CARTESIAN_POINT('Ctrl Pts',(1.6211138875,51.5979166676226,0.935950539335165));
#8842=CARTESIAN_POINT('Ctrl Pts',(0.810556943750001,51.5395833342893,1.40392580900275));
#8843=CARTESIAN_POINT('Ctrl Pts',(3.43862649647115E-16,51.4812500009559,
1.87190107867033));
#8844=CARTESIAN_POINT('Ctrl Pts',(-0.810556943749999,51.4229166676226,1.40392580900275));
#8845=CARTESIAN_POINT('Ctrl Pts',(-1.6211138875,51.3645833342893,0.935950539335167));
#8846=CARTESIAN_POINT('Ctrl Pts',(-1.6211138875,51.3062500009559,0.));
#8847=CARTESIAN_POINT('Ctrl Pts',(-1.6211138875,51.2479166676226,-0.935950539335166));
#8848=CARTESIAN_POINT('Ctrl Pts',(-0.81055694375,51.1895833342893,-1.40392580900275));
#8849=CARTESIAN_POINT('Ctrl Pts',(-1.14620883215705E-16,51.1312500009559,
-1.87190107867033));
#8850=CARTESIAN_POINT('Ctrl Pts',(0.81055694375,51.0729166676226,-1.40392580900275));
#8851=CARTESIAN_POINT('Ctrl Pts',(1.6211138875,51.0145833342893,-0.935950539335166));
#8852=CARTESIAN_POINT('Ctrl Pts',(1.6211138875,50.9562500009559,-1.9852919333802E-16));
#8853=CARTESIAN_POINT('Ctrl Pts',(1.6211138875,50.8979166676226,0.935950539335165));
#8854=CARTESIAN_POINT('Ctrl Pts',(0.810556943750001,50.8395833342893,1.40392580900275));
#8855=CARTESIAN_POINT('Ctrl Pts',(3.43862649647115E-16,50.7812500009559,
1.87190107867033));
#8856=CARTESIAN_POINT('Ctrl Pts',(-0.810556943749999,50.7229166676226,1.40392580900275));
#8857=CARTESIAN_POINT('Ctrl Pts',(-1.6211138875,50.6645833342893,0.935950539335167));
#8858=CARTESIAN_POINT('Ctrl Pts',(-1.6211138875,50.6062500009559,0.));
#8859=CARTESIAN_POINT('Ctrl Pts',(-1.6211138875,50.5479166676226,-0.935950539335166));
#8860=CARTESIAN_POINT('Ctrl Pts',(-0.81055694375,50.4895833342893,-1.40392580900275));
#8861=CARTESIAN_POINT('Ctrl Pts',(-1.14620883215705E-16,50.4312500009559,
-1.87190107867033));
#8862=CARTESIAN_POINT('Ctrl Pts',(0.81055694375,50.3729166676226,-1.40392580900275));
#8863=CARTESIAN_POINT('Ctrl Pts',(1.6211138875,50.3145833342893,-0.935950539335166));
#8864=CARTESIAN_POINT('Ctrl Pts',(1.6211138875,50.2562500009559,-1.9852919333802E-16));
#8865=CARTESIAN_POINT('Ctrl Pts',(1.6211138875,50.1979166676226,0.935950539335165));
#8866=CARTESIAN_POINT('Ctrl Pts',(0.810556943750001,50.1395833342893,1.40392580900275));
#8867=CARTESIAN_POINT('Ctrl Pts',(3.43862649647115E-16,50.0812500009559,
1.87190107867033));
#8868=CARTESIAN_POINT('Ctrl Pts',(-0.810556943749999,50.0229166676226,1.40392580900275));
#8869=CARTESIAN_POINT('Ctrl Pts',(-1.6211138875,49.9645833342893,0.935950539335167));
#8870=CARTESIAN_POINT('Ctrl Pts',(-1.6211138875,49.9062500009559,0.));
#8871=CARTESIAN_POINT('Ctrl Pts',(-1.6211138875,49.8479166676226,-0.935950539335166));
#8872=CARTESIAN_POINT('Ctrl Pts',(-0.81055694375,49.7895833342893,-1.40392580900275));
#8873=CARTESIAN_POINT('Ctrl Pts',(-1.14620883215705E-16,49.7312500009559,
-1.87190107867033));
#8874=CARTESIAN_POINT('Ctrl Pts',(0.81055694375,49.6729166676226,-1.40392580900275));
#8875=CARTESIAN_POINT('Ctrl Pts',(1.6211138875,49.6145833342893,-0.935950539335166));
#8876=CARTESIAN_POINT('Ctrl Pts',(1.6211138875,49.5562500009559,-1.9852919333802E-16));
#8877=CARTESIAN_POINT('Ctrl Pts',(1.6211138875,49.4979166676226,0.935950539335165));
#8878=CARTESIAN_POINT('Ctrl Pts',(0.810556943750001,49.4395833342893,1.40392580900275));
#8879=CARTESIAN_POINT('Ctrl Pts',(3.43862649647115E-16,49.3812500009559,
1.87190107867033));
#8880=CARTESIAN_POINT('Ctrl Pts',(-0.810556943749999,49.3229166676226,1.40392580900275));
#8881=CARTESIAN_POINT('Ctrl Pts',(-1.6211138875,49.2645833342893,0.935950539335167));
#8882=CARTESIAN_POINT('Ctrl Pts',(-1.6211138875,49.2062500009559,0.));
#8883=CARTESIAN_POINT('Ctrl Pts',(-1.6211138875,49.1479166676226,-0.935950539335166));
#8884=CARTESIAN_POINT('Ctrl Pts',(-0.81055694375,49.0895833342893,-1.40392580900275));
#8885=CARTESIAN_POINT('Ctrl Pts',(-1.14620883215705E-16,49.0312500009559,
-1.87190107867033));
#8886=CARTESIAN_POINT('Ctrl Pts',(0.81055694375,48.9729166676226,-1.40392580900275));
#8887=CARTESIAN_POINT('Ctrl Pts',(1.6211138875,48.9145833342893,-0.935950539335166));
#8888=CARTESIAN_POINT('Ctrl Pts',(1.6211138875,48.8562500009559,-1.9852919333802E-16));
#8889=CARTESIAN_POINT('Ctrl Pts',(1.6211138875,48.7979166676226,0.935950539335165));
#8890=CARTESIAN_POINT('Ctrl Pts',(0.810556943750001,48.7395833342893,1.40392580900275));
#8891=CARTESIAN_POINT('Ctrl Pts',(3.43862649647115E-16,48.6812500009559,
1.87190107867033));
#8892=CARTESIAN_POINT('Ctrl Pts',(-0.810556943749999,48.6229166676226,1.40392580900275));
#8893=CARTESIAN_POINT('Ctrl Pts',(-1.6211138875,48.5645833342893,0.935950539335167));
#8894=CARTESIAN_POINT('Ctrl Pts',(-1.6211138875,48.5062500009559,0.));
#8895=CARTESIAN_POINT('Ctrl Pts',(-1.6211138875,48.4479166676226,-0.935950539335166));
#8896=CARTESIAN_POINT('Ctrl Pts',(-0.81055694375,48.3895833342893,-1.40392580900275));
#8897=CARTESIAN_POINT('Ctrl Pts',(-1.14620883215705E-16,48.3312500009559,
-1.87190107867033));
#8898=CARTESIAN_POINT('Ctrl Pts',(0.81055694375,48.2729166676226,-1.40392580900275));
#8899=CARTESIAN_POINT('Ctrl Pts',(1.6211138875,48.2145833342893,-0.935950539335166));
#8900=CARTESIAN_POINT('Ctrl Pts',(1.6211138875,48.1562500009559,-1.9852919333802E-16));
#8901=CARTESIAN_POINT('Ctrl Pts',(1.6211138875,48.0979166676226,0.935950539335165));
#8902=CARTESIAN_POINT('Ctrl Pts',(0.810556943750001,48.0395833342893,1.40392580900275));
#8903=CARTESIAN_POINT('Ctrl Pts',(3.43862649647115E-16,47.9812500009559,
1.87190107867033));
#8904=CARTESIAN_POINT('Ctrl Pts',(-0.810556943749999,47.9229166676226,1.40392580900275));
#8905=CARTESIAN_POINT('Ctrl Pts',(-1.6211138875,47.8645833342893,0.935950539335167));
#8906=CARTESIAN_POINT('Ctrl Pts',(-1.6211138875,47.8062500009559,0.));
#8907=CARTESIAN_POINT('Ctrl Pts',(-1.6211138875,47.7479166676226,-0.935950539335166));
#8908=CARTESIAN_POINT('Ctrl Pts',(-0.81055694375,47.6895833342893,-1.40392580900275));
#8909=CARTESIAN_POINT('Ctrl Pts',(-1.14620883215705E-16,47.6312500009559,
-1.87190107867033));
#8910=CARTESIAN_POINT('Ctrl Pts',(0.81055694375,47.5729166676226,-1.40392580900275));
#8911=CARTESIAN_POINT('Ctrl Pts',(1.6211138875,47.5145833342893,-0.935950539335166));
#8912=CARTESIAN_POINT('Ctrl Pts',(1.6211138875,47.4562500009559,-1.9852919333802E-16));
#8913=CARTESIAN_POINT('Ctrl Pts',(1.6211138875,47.3979166676226,0.935950539335165));
#8914=CARTESIAN_POINT('Ctrl Pts',(0.810556943750001,47.3395833342893,1.40392580900275));
#8915=CARTESIAN_POINT('Ctrl Pts',(3.43862649647115E-16,47.2812500009559,
1.87190107867033));
#8916=CARTESIAN_POINT('Ctrl Pts',(-0.810556943749999,47.2229166676226,1.40392580900275));
#8917=CARTESIAN_POINT('Ctrl Pts',(-1.6211138875,47.1645833342893,0.935950539335167));
#8918=CARTESIAN_POINT('Ctrl Pts',(-1.6211138875,47.1062500009559,0.));
#8919=CARTESIAN_POINT('Ctrl Pts',(-1.6211138875,47.0479166676226,-0.935950539335166));
#8920=CARTESIAN_POINT('Ctrl Pts',(-0.81055694375,46.9895833342893,-1.40392580900275));
#8921=CARTESIAN_POINT('Ctrl Pts',(-1.14620883215705E-16,46.9312500009559,
-1.87190107867033));
#8922=CARTESIAN_POINT('Ctrl Pts',(0.81055694375,46.8729166676226,-1.40392580900275));
#8923=CARTESIAN_POINT('Ctrl Pts',(1.6211138875,46.8145833342893,-0.935950539335166));
#8924=CARTESIAN_POINT('Ctrl Pts',(1.6211138875,46.7562500009559,-1.9852919333802E-16));
#8925=CARTESIAN_POINT('Ctrl Pts',(1.6211138875,46.6979166676226,0.935950539335165));
#8926=CARTESIAN_POINT('Ctrl Pts',(0.810556943750001,46.6395833342893,1.40392580900275));
#8927=CARTESIAN_POINT('Ctrl Pts',(3.43862649647115E-16,46.5812500009559,
1.87190107867033));
#8928=CARTESIAN_POINT('Ctrl Pts',(-0.810556943749999,46.5229166676226,1.40392580900275));
#8929=CARTESIAN_POINT('Ctrl Pts',(-1.6211138875,46.4645833342893,0.935950539335167));
#8930=CARTESIAN_POINT('Ctrl Pts',(-1.6211138875,46.4062500009559,0.));
#8931=CARTESIAN_POINT('Ctrl Pts',(-1.6211138875,46.3479166676226,-0.935950539335166));
#8932=CARTESIAN_POINT('Ctrl Pts',(-0.81055694375,46.2895833342893,-1.40392580900275));
#8933=CARTESIAN_POINT('Ctrl Pts',(-1.14620883215705E-16,46.2312500009559,
-1.87190107867033));
#8934=CARTESIAN_POINT('Ctrl Pts',(0.81055694375,46.1729166676226,-1.40392580900275));
#8935=CARTESIAN_POINT('Ctrl Pts',(1.6211138875,46.1145833342893,-0.935950539335166));
#8936=CARTESIAN_POINT('Ctrl Pts',(1.6211138875,46.0562500009559,-1.9852919333802E-16));
#8937=CARTESIAN_POINT('Ctrl Pts',(1.6211138875,45.9979166676226,0.935950539335165));
#8938=CARTESIAN_POINT('Ctrl Pts',(0.810556943750001,45.9395833342893,1.40392580900275));
#8939=CARTESIAN_POINT('Ctrl Pts',(3.43862649647115E-16,45.8812500009559,
1.87190107867033));
#8940=CARTESIAN_POINT('Ctrl Pts',(-0.810556943749999,45.8229166676226,1.40392580900275));
#8941=CARTESIAN_POINT('Ctrl Pts',(-1.6211138875,45.7645833342893,0.935950539335167));
#8942=CARTESIAN_POINT('Ctrl Pts',(-1.6211138875,45.7062500009559,0.));
#8943=CARTESIAN_POINT('Ctrl Pts',(-1.6211138875,45.6479166676226,-0.935950539335166));
#8944=CARTESIAN_POINT('Ctrl Pts',(-0.81055694375,45.5895833342893,-1.40392580900275));
#8945=CARTESIAN_POINT('Ctrl Pts',(-1.14620883215705E-16,45.5312500009559,
-1.87190107867033));
#8946=CARTESIAN_POINT('Ctrl Pts',(0.81055694375,45.4729166676226,-1.40392580900275));
#8947=CARTESIAN_POINT('Ctrl Pts',(1.6211138875,45.4145833342893,-0.935950539335166));
#8948=CARTESIAN_POINT('Ctrl Pts',(1.6211138875,45.3562500009559,-1.9852919333802E-16));
#8949=CARTESIAN_POINT('Ctrl Pts',(1.6211138875,45.2979166676226,0.935950539335165));
#8950=CARTESIAN_POINT('Ctrl Pts',(0.810556943750001,45.2395833342893,1.40392580900275));
#8951=CARTESIAN_POINT('Ctrl Pts',(3.43862649647115E-16,45.1812500009559,
1.87190107867033));
#8952=CARTESIAN_POINT('Ctrl Pts',(-0.810556943749999,45.1229166676226,1.40392580900275));
#8953=CARTESIAN_POINT('Ctrl Pts',(-1.6211138875,45.0645833342893,0.935950539335167));
#8954=CARTESIAN_POINT('Ctrl Pts',(-1.6211138875,45.0062500009559,0.));
#8955=CARTESIAN_POINT('Ctrl Pts',(-1.6211138875,44.9479166676226,-0.935950539335166));
#8956=CARTESIAN_POINT('Ctrl Pts',(-0.81055694375,44.8895833342893,-1.40392580900275));
#8957=CARTESIAN_POINT('Ctrl Pts',(-1.14620883215705E-16,44.8312500009559,
-1.87190107867033));
#8958=CARTESIAN_POINT('Ctrl Pts',(0.81055694375,44.7729166676226,-1.40392580900275));
#8959=CARTESIAN_POINT('Ctrl Pts',(1.6211138875,44.7145833342893,-0.935950539335166));
#8960=CARTESIAN_POINT('Ctrl Pts',(1.6211138875,44.6562500009559,-1.9852919333802E-16));
#8961=CARTESIAN_POINT('Ctrl Pts',(1.6211138875,44.5979166676226,0.935950539335165));
#8962=CARTESIAN_POINT('Ctrl Pts',(0.810556943750001,44.5395833342893,1.40392580900275));
#8963=CARTESIAN_POINT('Ctrl Pts',(3.43862649647115E-16,44.4812500009559,
1.87190107867033));
#8964=CARTESIAN_POINT('Ctrl Pts',(-0.810556943749999,44.4229166676226,1.40392580900275));
#8965=CARTESIAN_POINT('Ctrl Pts',(-1.6211138875,44.3645833342893,0.935950539335167));
#8966=CARTESIAN_POINT('Ctrl Pts',(-1.6211138875,44.3062500009559,0.));
#8967=CARTESIAN_POINT('Ctrl Pts',(-1.6211138875,44.2479166676226,-0.935950539335166));
#8968=CARTESIAN_POINT('Ctrl Pts',(-0.81055694375,44.1895833342893,-1.40392580900275));
#8969=CARTESIAN_POINT('Ctrl Pts',(-1.14620883215705E-16,44.1312500009559,
-1.87190107867033));
#8970=CARTESIAN_POINT('Ctrl Pts',(0.81055694375,44.0729166676226,-1.40392580900275));
#8971=CARTESIAN_POINT('Ctrl Pts',(1.6211138875,44.0145833342893,-0.935950539335166));
#8972=CARTESIAN_POINT('Ctrl Pts',(1.6211138875,43.9562500009559,-1.9852919333802E-16));
#8973=CARTESIAN_POINT('Ctrl Pts',(1.6211138875,43.8979166676226,0.935950539335165));
#8974=CARTESIAN_POINT('Ctrl Pts',(0.810556943750001,43.8395833342893,1.40392580900275));
#8975=CARTESIAN_POINT('Ctrl Pts',(3.43862649647115E-16,43.7812500009559,
1.87190107867033));
#8976=CARTESIAN_POINT('Ctrl Pts',(-0.810556943749999,43.7229166676226,1.40392580900275));
#8977=CARTESIAN_POINT('Ctrl Pts',(-1.6211138875,43.6645833342893,0.935950539335167));
#8978=CARTESIAN_POINT('Ctrl Pts',(-1.6211138875,43.6062500009559,0.));
#8979=CARTESIAN_POINT('Ctrl Pts',(-1.6211138875,43.5479166676226,-0.935950539335166));
#8980=CARTESIAN_POINT('Ctrl Pts',(-0.81055694375,43.4895833342893,-1.40392580900275));
#8981=CARTESIAN_POINT('Ctrl Pts',(-1.14620883215705E-16,43.4312500009559,
-1.87190107867033));
#8982=CARTESIAN_POINT('Ctrl Pts',(0.81055694375,43.3729166676226,-1.40392580900275));
#8983=CARTESIAN_POINT('Ctrl Pts',(1.6211138875,43.3145833342893,-0.935950539335166));
#8984=CARTESIAN_POINT('Ctrl Pts',(1.6211138875,43.2562500009559,-1.9852919333802E-16));
#8985=CARTESIAN_POINT('Ctrl Pts',(1.6211138875,43.1979166676226,0.935950539335165));
#8986=CARTESIAN_POINT('Ctrl Pts',(0.810556943750001,43.1395833342893,1.40392580900275));
#8987=CARTESIAN_POINT('Ctrl Pts',(3.43862649647115E-16,43.0812500009559,
1.87190107867033));
#8988=CARTESIAN_POINT('Ctrl Pts',(-0.810556943749999,43.0229166676226,1.40392580900275));
#8989=CARTESIAN_POINT('Ctrl Pts',(-1.6211138875,42.9645833342893,0.935950539335167));
#8990=CARTESIAN_POINT('Ctrl Pts',(-1.6211138875,42.9062500009559,0.));
#8991=CARTESIAN_POINT('Ctrl Pts',(-1.6211138875,42.8479166676226,-0.935950539335166));
#8992=CARTESIAN_POINT('Ctrl Pts',(-0.81055694375,42.7895833342893,-1.40392580900275));
#8993=CARTESIAN_POINT('Ctrl Pts',(-1.14620883215705E-16,42.7312500009559,
-1.87190107867033));
#8994=CARTESIAN_POINT('Ctrl Pts',(0.81055694375,42.6729166676226,-1.40392580900275));
#8995=CARTESIAN_POINT('Ctrl Pts',(1.6211138875,42.6145833342893,-0.935950539335166));
#8996=CARTESIAN_POINT('Ctrl Pts',(1.6211138875,42.5562500009559,-1.9852919333802E-16));
#8997=CARTESIAN_POINT('Ctrl Pts',(1.6211138875,42.4979166676226,0.935950539335165));
#8998=CARTESIAN_POINT('Ctrl Pts',(0.810556943750001,42.4395833342893,1.40392580900275));
#8999=CARTESIAN_POINT('Ctrl Pts',(3.43862649647115E-16,42.3812500009559,
1.87190107867033));
#9000=CARTESIAN_POINT('Ctrl Pts',(-0.810556943749999,42.3229166676226,1.40392580900275));
#9001=CARTESIAN_POINT('Ctrl Pts',(-1.6211138875,42.2645833342893,0.935950539335167));
#9002=CARTESIAN_POINT('Ctrl Pts',(-1.6211138875,42.2062500009559,0.));
#9003=CARTESIAN_POINT('Ctrl Pts',(-1.6211138875,42.1479166676226,-0.935950539335166));
#9004=CARTESIAN_POINT('Ctrl Pts',(-0.81055694375,42.0895833342893,-1.40392580900275));
#9005=CARTESIAN_POINT('Ctrl Pts',(-1.14620883215705E-16,42.0312500009559,
-1.87190107867033));
#9006=CARTESIAN_POINT('Ctrl Pts',(0.81055694375,41.9729166676226,-1.40392580900275));
#9007=CARTESIAN_POINT('Ctrl Pts',(1.6211138875,41.9145833342893,-0.935950539335166));
#9008=CARTESIAN_POINT('Ctrl Pts',(1.6211138875,41.8562500009559,-1.9852919333802E-16));
#9009=CARTESIAN_POINT('Ctrl Pts',(1.6211138875,41.7979166676226,0.935950539335165));
#9010=CARTESIAN_POINT('Ctrl Pts',(0.810556943750001,41.7395833342893,1.40392580900275));
#9011=CARTESIAN_POINT('Ctrl Pts',(3.43862649647115E-16,41.6812500009559,
1.87190107867033));
#9012=CARTESIAN_POINT('Ctrl Pts',(-0.810556943749999,41.6229166676226,1.40392580900275));
#9013=CARTESIAN_POINT('Ctrl Pts',(-1.6211138875,41.5645833342893,0.935950539335167));
#9014=CARTESIAN_POINT('Ctrl Pts',(-1.6211138875,41.5062500009559,0.));
#9015=CARTESIAN_POINT('Ctrl Pts',(-1.6211138875,41.4479166676226,-0.935950539335166));
#9016=CARTESIAN_POINT('Ctrl Pts',(-0.81055694375,41.3895833342893,-1.40392580900275));
#9017=CARTESIAN_POINT('Ctrl Pts',(-1.14620883215705E-16,41.3312500009559,
-1.87190107867033));
#9018=CARTESIAN_POINT('Ctrl Pts',(0.81055694375,41.2729166676226,-1.40392580900275));
#9019=CARTESIAN_POINT('Ctrl Pts',(1.6211138875,41.2145833342893,-0.935950539335166));
#9020=CARTESIAN_POINT('Ctrl Pts',(1.6211138875,41.1562500009559,-1.9852919333802E-16));
#9021=CARTESIAN_POINT('Ctrl Pts',(1.6211138875,41.0979166676226,0.935950539335165));
#9022=CARTESIAN_POINT('Ctrl Pts',(0.810556943750001,41.0395833342893,1.40392580900275));
#9023=CARTESIAN_POINT('Ctrl Pts',(3.43862649647115E-16,40.9812500009559,
1.87190107867033));
#9024=CARTESIAN_POINT('Ctrl Pts',(-0.810556943749999,40.9229166676226,1.40392580900275));
#9025=CARTESIAN_POINT('Ctrl Pts',(-1.6211138875,40.8645833342893,0.935950539335167));
#9026=CARTESIAN_POINT('Ctrl Pts',(-1.6211138875,40.8062500009559,0.));
#9027=CARTESIAN_POINT('Ctrl Pts',(-1.6211138875,40.7479166676226,-0.935950539335166));
#9028=CARTESIAN_POINT('Ctrl Pts',(-0.81055694375,40.6895833342893,-1.40392580900275));
#9029=CARTESIAN_POINT('Ctrl Pts',(-1.14620883215705E-16,40.6312500009559,
-1.87190107867033));
#9030=CARTESIAN_POINT('Ctrl Pts',(0.81055694375,40.5729166676226,-1.40392580900275));
#9031=CARTESIAN_POINT('Ctrl Pts',(1.6211138875,40.5145833342893,-0.935950539335166));
#9032=CARTESIAN_POINT('Ctrl Pts',(1.6211138875,40.4562500009559,-1.9852919333802E-16));
#9033=CARTESIAN_POINT('Ctrl Pts',(1.6211138875,40.3979166676226,0.935950539335165));
#9034=CARTESIAN_POINT('Ctrl Pts',(0.810556943750001,40.3395833342893,1.40392580900275));
#9035=CARTESIAN_POINT('Ctrl Pts',(3.43862649647115E-16,40.2812500009559,
1.87190107867033));
#9036=CARTESIAN_POINT('Ctrl Pts',(-0.810556943749999,40.2229166676226,1.40392580900275));
#9037=CARTESIAN_POINT('Ctrl Pts',(-1.6211138875,40.1645833342893,0.935950539335167));
#9038=CARTESIAN_POINT('Ctrl Pts',(-1.6211138875,40.1062500009559,0.));
#9039=CARTESIAN_POINT('Ctrl Pts',(-1.6211138875,40.0479166676226,-0.935950539335166));
#9040=CARTESIAN_POINT('Ctrl Pts',(-0.81055694375,39.9895833342893,-1.40392580900275));
#9041=CARTESIAN_POINT('Ctrl Pts',(-1.14620883215705E-16,39.9312500009559,
-1.87190107867033));
#9042=CARTESIAN_POINT('Ctrl Pts',(0.81055694375,39.8729166676226,-1.40392580900275));
#9043=CARTESIAN_POINT('Ctrl Pts',(1.6211138875,39.8145833342893,-0.935950539335166));
#9044=CARTESIAN_POINT('Ctrl Pts',(1.6211138875,39.7562500009559,-1.9852919333802E-16));
#9045=CARTESIAN_POINT('Ctrl Pts',(1.6211138875,39.6979166676226,0.935950539335165));
#9046=CARTESIAN_POINT('Ctrl Pts',(0.810556943750001,39.6395833342893,1.40392580900275));
#9047=CARTESIAN_POINT('Ctrl Pts',(3.43862649647115E-16,39.5812500009559,
1.87190107867033));
#9048=CARTESIAN_POINT('Ctrl Pts',(-0.810556943749999,39.5229166676226,1.40392580900275));
#9049=CARTESIAN_POINT('Ctrl Pts',(-1.6211138875,39.4645833342893,0.935950539335167));
#9050=CARTESIAN_POINT('Ctrl Pts',(-1.6211138875,39.4062500009559,0.));
#9051=CARTESIAN_POINT('Ctrl Pts',(-1.6211138875,39.3479166676226,-0.935950539335166));
#9052=CARTESIAN_POINT('Ctrl Pts',(-0.81055694375,39.2895833342893,-1.40392580900275));
#9053=CARTESIAN_POINT('Ctrl Pts',(-1.14620883215705E-16,39.2312500009559,
-1.87190107867033));
#9054=CARTESIAN_POINT('Ctrl Pts',(0.81055694375,39.1729166676226,-1.40392580900275));
#9055=CARTESIAN_POINT('Ctrl Pts',(1.6211138875,39.1145833342893,-0.935950539335166));
#9056=CARTESIAN_POINT('Ctrl Pts',(1.6211138875,39.0562500009559,-1.9852919333802E-16));
#9057=CARTESIAN_POINT('Ctrl Pts',(1.6211138875,38.9979166676226,0.935950539335165));
#9058=CARTESIAN_POINT('Ctrl Pts',(0.810556943750001,38.9395833342893,1.40392580900275));
#9059=CARTESIAN_POINT('Ctrl Pts',(3.43862649647115E-16,38.8812500009559,
1.87190107867033));
#9060=CARTESIAN_POINT('Ctrl Pts',(-0.810556943749999,38.8229166676226,1.40392580900275));
#9061=CARTESIAN_POINT('Ctrl Pts',(-1.6211138875,38.7645833342893,0.935950539335167));
#9062=CARTESIAN_POINT('Ctrl Pts',(-1.6211138875,38.7062500009559,0.));
#9063=CARTESIAN_POINT('Ctrl Pts',(-1.6211138875,38.6479166676226,-0.935950539335166));
#9064=CARTESIAN_POINT('Ctrl Pts',(-0.81055694375,38.5895833342893,-1.40392580900275));
#9065=CARTESIAN_POINT('Ctrl Pts',(-1.14620883215705E-16,38.5312500009559,
-1.87190107867033));
#9066=CARTESIAN_POINT('Ctrl Pts',(0.81055694375,38.4729166676226,-1.40392580900275));
#9067=CARTESIAN_POINT('Ctrl Pts',(1.6211138875,38.4145833342893,-0.935950539335166));
#9068=CARTESIAN_POINT('Ctrl Pts',(1.6211138875,38.3562500009559,-1.9852919333802E-16));
#9069=CARTESIAN_POINT('Ctrl Pts',(1.6211138875,38.2979166676226,0.935950539335165));
#9070=CARTESIAN_POINT('Ctrl Pts',(0.810556943750001,38.2395833342893,1.40392580900275));
#9071=CARTESIAN_POINT('Ctrl Pts',(3.43862649647115E-16,38.1812500009559,
1.87190107867033));
#9072=CARTESIAN_POINT('Ctrl Pts',(-0.810556943749999,38.1229166676226,1.40392580900275));
#9073=CARTESIAN_POINT('Ctrl Pts',(-1.6211138875,38.0645833342893,0.935950539335167));
#9074=CARTESIAN_POINT('Ctrl Pts',(-1.6211138875,38.0062500009559,0.));
#9075=CARTESIAN_POINT('Ctrl Pts',(-1.6211138875,37.9479166676226,-0.935950539335166));
#9076=CARTESIAN_POINT('Ctrl Pts',(-0.81055694375,37.8895833342893,-1.40392580900275));
#9077=CARTESIAN_POINT('Ctrl Pts',(-1.14620883215705E-16,37.8312500009559,
-1.87190107867033));
#9078=CARTESIAN_POINT('Ctrl Pts',(0.81055694375,37.7729166676226,-1.40392580900275));
#9079=CARTESIAN_POINT('Ctrl Pts',(1.6211138875,37.7145833342893,-0.935950539335166));
#9080=CARTESIAN_POINT('Ctrl Pts',(1.6211138875,37.6562500009559,-1.9852919333802E-16));
#9081=CARTESIAN_POINT('Ctrl Pts',(1.6211138875,37.5979166676226,0.935950539335165));
#9082=CARTESIAN_POINT('Ctrl Pts',(0.810556943750001,37.5395833342893,1.40392580900275));
#9083=CARTESIAN_POINT('Ctrl Pts',(3.43862649647115E-16,37.4812500009559,
1.87190107867033));
#9084=CARTESIAN_POINT('Ctrl Pts',(-0.810556943749999,37.4229166676226,1.40392580900275));
#9085=CARTESIAN_POINT('Ctrl Pts',(-1.6211138875,37.3645833342893,0.935950539335167));
#9086=CARTESIAN_POINT('Ctrl Pts',(-1.6211138875,37.3062500009559,0.));
#9087=CARTESIAN_POINT('Ctrl Pts',(-1.6211138875,37.2479166676226,-0.935950539335166));
#9088=CARTESIAN_POINT('Ctrl Pts',(-0.81055694375,37.1895833342893,-1.40392580900275));
#9089=CARTESIAN_POINT('Ctrl Pts',(-1.14620883215705E-16,37.1312500009559,
-1.87190107867033));
#9090=CARTESIAN_POINT('Ctrl Pts',(0.81055694375,37.0729166676226,-1.40392580900275));
#9091=CARTESIAN_POINT('Ctrl Pts',(1.6211138875,37.0145833342893,-0.935950539335166));
#9092=CARTESIAN_POINT('Ctrl Pts',(1.6211138875,36.9562500009559,-1.9852919333802E-16));
#9093=CARTESIAN_POINT('Ctrl Pts',(1.6211138875,36.8979166676226,0.935950539335165));
#9094=CARTESIAN_POINT('Ctrl Pts',(0.810556943750001,36.8395833342893,1.40392580900275));
#9095=CARTESIAN_POINT('Ctrl Pts',(3.43862649647115E-16,36.7812500009559,
1.87190107867033));
#9096=CARTESIAN_POINT('Ctrl Pts',(-0.810556943749999,36.7229166676226,1.40392580900275));
#9097=CARTESIAN_POINT('Ctrl Pts',(-1.6211138875,36.6645833342893,0.935950539335167));
#9098=CARTESIAN_POINT('Ctrl Pts',(-1.6211138875,36.6062500009559,0.));
#9099=CARTESIAN_POINT('Ctrl Pts',(-1.6211138875,36.5479166676226,-0.935950539335166));
#9100=CARTESIAN_POINT('Ctrl Pts',(-0.81055694375,36.4895833342893,-1.40392580900275));
#9101=CARTESIAN_POINT('Ctrl Pts',(-1.14620883215705E-16,36.4312500009559,
-1.87190107867033));
#9102=CARTESIAN_POINT('Ctrl Pts',(0.81055694375,36.3729166676226,-1.40392580900275));
#9103=CARTESIAN_POINT('Ctrl Pts',(1.6211138875,36.3145833342893,-0.935950539335166));
#9104=CARTESIAN_POINT('Ctrl Pts',(1.6211138875,36.2562500009559,-1.9852919333802E-16));
#9105=CARTESIAN_POINT('Ctrl Pts',(1.6211138875,36.1979166676226,0.935950539335165));
#9106=CARTESIAN_POINT('Ctrl Pts',(0.810556943750001,36.1395833342893,1.40392580900275));
#9107=CARTESIAN_POINT('Ctrl Pts',(3.43862649647115E-16,36.0812500009559,
1.87190107867033));
#9108=CARTESIAN_POINT('Ctrl Pts',(-0.810556943749999,36.0229166676226,1.40392580900275));
#9109=CARTESIAN_POINT('Ctrl Pts',(-1.6211138875,35.9645833342893,0.935950539335167));
#9110=CARTESIAN_POINT('Ctrl Pts',(-1.6211138875,35.9062500009559,0.));
#9111=CARTESIAN_POINT('Ctrl Pts',(-1.6211138875,35.8479166676226,-0.935950539335166));
#9112=CARTESIAN_POINT('Ctrl Pts',(-0.81055694375,35.7895833342893,-1.40392580900275));
#9113=CARTESIAN_POINT('Ctrl Pts',(-1.14620883215705E-16,35.7312500009559,
-1.87190107867033));
#9114=CARTESIAN_POINT('Ctrl Pts',(0.81055694375,35.6729166676226,-1.40392580900275));
#9115=CARTESIAN_POINT('Ctrl Pts',(1.6211138875,35.6145833342893,-0.935950539335166));
#9116=CARTESIAN_POINT('Ctrl Pts',(1.6211138875,35.5562500009559,-1.9852919333802E-16));
#9117=CARTESIAN_POINT('Ctrl Pts',(1.6211138875,35.4979166676226,0.935950539335165));
#9118=CARTESIAN_POINT('Ctrl Pts',(0.810556943750001,35.4395833342893,1.40392580900275));
#9119=CARTESIAN_POINT('Ctrl Pts',(3.43862649647115E-16,35.3812500009559,
1.87190107867033));
#9120=CARTESIAN_POINT('Ctrl Pts',(-0.810556943749999,35.3229166676226,1.40392580900275));
#9121=CARTESIAN_POINT('Ctrl Pts',(-1.6211138875,35.2645833342893,0.935950539335167));
#9122=CARTESIAN_POINT('Ctrl Pts',(-1.6211138875,35.2062500009559,0.));
#9123=CARTESIAN_POINT('Ctrl Pts',(-1.6211138875,35.1479166676226,-0.935950539335166));
#9124=CARTESIAN_POINT('Ctrl Pts',(-0.81055694375,35.0895833342893,-1.40392580900275));
#9125=CARTESIAN_POINT('Ctrl Pts',(-1.14620883215705E-16,35.0312500009559,
-1.87190107867033));
#9126=CARTESIAN_POINT('Ctrl Pts',(0.81055694375,34.9729166676226,-1.40392580900275));
#9127=CARTESIAN_POINT('Ctrl Pts',(1.6211138875,34.9145833342893,-0.935950539335166));
#9128=CARTESIAN_POINT('Ctrl Pts',(1.6211138875,34.8562500009559,-1.9852919333802E-16));
#9129=CARTESIAN_POINT('Ctrl Pts',(1.6211138875,34.7979166676226,0.935950539335165));
#9130=CARTESIAN_POINT('Ctrl Pts',(0.810556943750001,34.7395833342893,1.40392580900275));
#9131=CARTESIAN_POINT('Ctrl Pts',(3.43862649647115E-16,34.6812500009559,
1.87190107867033));
#9132=CARTESIAN_POINT('Ctrl Pts',(-0.810556943749999,34.6229166676226,1.40392580900275));
#9133=CARTESIAN_POINT('Ctrl Pts',(-1.6211138875,34.5645833342893,0.935950539335167));
#9134=CARTESIAN_POINT('Ctrl Pts',(-1.6211138875,34.5062500009559,0.));
#9135=CARTESIAN_POINT('Ctrl Pts',(-1.6211138875,34.4479166676226,-0.935950539335166));
#9136=CARTESIAN_POINT('Ctrl Pts',(-0.81055694375,34.3895833342893,-1.40392580900275));
#9137=CARTESIAN_POINT('Ctrl Pts',(-1.14620883215705E-16,34.3312500009559,
-1.87190107867033));
#9138=CARTESIAN_POINT('Ctrl Pts',(0.81055694375,34.2729166676226,-1.40392580900275));
#9139=CARTESIAN_POINT('Ctrl Pts',(1.6211138875,34.2145833342893,-0.935950539335166));
#9140=CARTESIAN_POINT('Ctrl Pts',(1.6211138875,34.1562500009559,-1.9852919333802E-16));
#9141=CARTESIAN_POINT('Ctrl Pts',(1.6211138875,34.0979166676226,0.935950539335165));
#9142=CARTESIAN_POINT('Ctrl Pts',(0.810556943750001,34.0395833342893,1.40392580900275));
#9143=CARTESIAN_POINT('Ctrl Pts',(3.43862649647115E-16,33.9812500009559,
1.87190107867033));
#9144=CARTESIAN_POINT('Ctrl Pts',(-0.810556943749999,33.9229166676226,1.40392580900275));
#9145=CARTESIAN_POINT('Ctrl Pts',(-1.6211138875,33.8645833342893,0.935950539335167));
#9146=CARTESIAN_POINT('Ctrl Pts',(-1.6211138875,33.8062500009559,0.));
#9147=CARTESIAN_POINT('Ctrl Pts',(-1.6211138875,33.7479166676226,-0.935950539335166));
#9148=CARTESIAN_POINT('Ctrl Pts',(-0.81055694375,33.6895833342893,-1.40392580900275));
#9149=CARTESIAN_POINT('Ctrl Pts',(-1.14620883215705E-16,33.6312500009559,
-1.87190107867033));
#9150=CARTESIAN_POINT('Ctrl Pts',(0.81055694375,33.5729166676226,-1.40392580900275));
#9151=CARTESIAN_POINT('Ctrl Pts',(1.6211138875,33.5145833342893,-0.935950539335166));
#9152=CARTESIAN_POINT('Ctrl Pts',(1.6211138875,33.4562500009559,-1.9852919333802E-16));
#9153=CARTESIAN_POINT('Ctrl Pts',(1.6211138875,33.3979166676226,0.935950539335165));
#9154=CARTESIAN_POINT('Ctrl Pts',(0.810556943750001,33.3395833342893,1.40392580900275));
#9155=CARTESIAN_POINT('Ctrl Pts',(3.43862649647115E-16,33.2812500009559,
1.87190107867033));
#9156=CARTESIAN_POINT('Ctrl Pts',(-0.810556943749999,33.2229166676226,1.40392580900275));
#9157=CARTESIAN_POINT('Ctrl Pts',(-1.6211138875,33.1645833342893,0.935950539335167));
#9158=CARTESIAN_POINT('Ctrl Pts',(-1.6211138875,33.1062500009559,0.));
#9159=CARTESIAN_POINT('Ctrl Pts',(-1.6211138875,33.0479166676226,-0.935950539335166));
#9160=CARTESIAN_POINT('Ctrl Pts',(-0.81055694375,32.9895833342893,-1.40392580900275));
#9161=CARTESIAN_POINT('Ctrl Pts',(-1.14620883215705E-16,32.9312500009559,
-1.87190107867033));
#9162=CARTESIAN_POINT('Ctrl Pts',(0.81055694375,32.8729166676226,-1.40392580900275));
#9163=CARTESIAN_POINT('Ctrl Pts',(1.6211138875,32.8145833342893,-0.935950539335166));
#9164=CARTESIAN_POINT('Ctrl Pts',(1.6211138875,32.7562500009559,-1.9852919333802E-16));
#9165=CARTESIAN_POINT('Ctrl Pts',(1.6211138875,32.6979166676226,0.935950539335165));
#9166=CARTESIAN_POINT('Ctrl Pts',(0.810556943750001,32.6395833342893,1.40392580900275));
#9167=CARTESIAN_POINT('Ctrl Pts',(3.43862649647115E-16,32.5812500009559,
1.87190107867033));
#9168=CARTESIAN_POINT('Ctrl Pts',(-0.810556943749999,32.5229166676226,1.40392580900275));
#9169=CARTESIAN_POINT('Ctrl Pts',(-1.6211138875,32.4645833342893,0.935950539335167));
#9170=CARTESIAN_POINT('Ctrl Pts',(-1.6211138875,32.4062500009559,0.));
#9171=CARTESIAN_POINT('Ctrl Pts',(-1.6211138875,32.3479166676226,-0.935950539335166));
#9172=CARTESIAN_POINT('Ctrl Pts',(-0.81055694375,32.2895833342893,-1.40392580900275));
#9173=CARTESIAN_POINT('Ctrl Pts',(-1.14620883215705E-16,32.2312500009559,
-1.87190107867033));
#9174=CARTESIAN_POINT('Ctrl Pts',(0.81055694375,32.1729166676226,-1.40392580900275));
#9175=CARTESIAN_POINT('Ctrl Pts',(1.6211138875,32.1145833342893,-0.935950539335166));
#9176=CARTESIAN_POINT('Ctrl Pts',(1.6211138875,32.0562500009559,-1.9852919333802E-16));
#9177=CARTESIAN_POINT('Ctrl Pts',(1.6211138875,31.9979166676226,0.935950539335165));
#9178=CARTESIAN_POINT('Ctrl Pts',(0.810556943750001,31.9395833342893,1.40392580900275));
#9179=CARTESIAN_POINT('Ctrl Pts',(3.43862649647115E-16,31.8812500009559,
1.87190107867033));
#9180=CARTESIAN_POINT('Ctrl Pts',(-0.810556943749999,31.8229166676226,1.40392580900275));
#9181=CARTESIAN_POINT('Ctrl Pts',(-1.6211138875,31.7645833342893,0.935950539335167));
#9182=CARTESIAN_POINT('Ctrl Pts',(-1.6211138875,31.7062500009559,0.));
#9183=CARTESIAN_POINT('Ctrl Pts',(-1.6211138875,31.6479166676226,-0.935950539335166));
#9184=CARTESIAN_POINT('Ctrl Pts',(-0.81055694375,31.5895833342893,-1.40392580900275));
#9185=CARTESIAN_POINT('Ctrl Pts',(-1.14620883215705E-16,31.5312500009559,
-1.87190107867033));
#9186=CARTESIAN_POINT('Ctrl Pts',(0.81055694375,31.4729166676226,-1.40392580900275));
#9187=CARTESIAN_POINT('Ctrl Pts',(1.6211138875,31.4145833342893,-0.935950539335166));
#9188=CARTESIAN_POINT('Ctrl Pts',(1.6211138875,31.3562500009559,-1.9852919333802E-16));
#9189=CARTESIAN_POINT('Ctrl Pts',(1.6211138875,31.2979166676226,0.935950539335165));
#9190=CARTESIAN_POINT('Ctrl Pts',(0.810556943750001,31.2395833342893,1.40392580900275));
#9191=CARTESIAN_POINT('Ctrl Pts',(3.43862649647115E-16,31.1812500009559,
1.87190107867033));
#9192=CARTESIAN_POINT('Ctrl Pts',(-0.810556943749999,31.1229166676226,1.40392580900275));
#9193=CARTESIAN_POINT('Ctrl Pts',(-1.6211138875,31.0645833342893,0.935950539335167));
#9194=CARTESIAN_POINT('Ctrl Pts',(-1.6211138875,31.0062500009559,0.));
#9195=CARTESIAN_POINT('Ctrl Pts',(-1.6211138875,30.9479166676226,-0.935950539335166));
#9196=CARTESIAN_POINT('Ctrl Pts',(-0.81055694375,30.8895833342893,-1.40392580900275));
#9197=CARTESIAN_POINT('Ctrl Pts',(-1.14620883215705E-16,30.8312500009559,
-1.87190107867033));
#9198=CARTESIAN_POINT('Ctrl Pts',(0.81055694375,30.7729166676226,-1.40392580900275));
#9199=CARTESIAN_POINT('Ctrl Pts',(1.6211138875,30.7145833342893,-0.935950539335166));
#9200=CARTESIAN_POINT('Ctrl Pts',(1.6211138875,30.6562500009559,-1.9852919333802E-16));
#9201=CARTESIAN_POINT('Ctrl Pts',(1.6211138875,30.5979166676226,0.935950539335165));
#9202=CARTESIAN_POINT('Ctrl Pts',(0.810556943750001,30.5395833342893,1.40392580900275));
#9203=CARTESIAN_POINT('Ctrl Pts',(3.43862649647115E-16,30.4812500009559,
1.87190107867033));
#9204=CARTESIAN_POINT('Ctrl Pts',(-0.810556943749999,30.4229166676226,1.40392580900275));
#9205=CARTESIAN_POINT('Ctrl Pts',(-1.6211138875,30.3645833342893,0.935950539335167));
#9206=CARTESIAN_POINT('Ctrl Pts',(-1.6211138875,30.3062500009559,0.));
#9207=CARTESIAN_POINT('Ctrl Pts',(-1.6211138875,30.2479166676226,-0.935950539335166));
#9208=CARTESIAN_POINT('Ctrl Pts',(-0.81055694375,30.1895833342893,-1.40392580900275));
#9209=CARTESIAN_POINT('Ctrl Pts',(-1.14620883215705E-16,30.1312500009559,
-1.87190107867033));
#9210=CARTESIAN_POINT('Ctrl Pts',(0.81055694375,30.0729166676226,-1.40392580900275));
#9211=CARTESIAN_POINT('Ctrl Pts',(1.6211138875,30.0145833342893,-0.935950539335166));
#9212=CARTESIAN_POINT('Ctrl Pts',(1.6211138875,29.9562500009559,-1.9852919333802E-16));
#9213=CARTESIAN_POINT('Ctrl Pts',(1.6211138875,29.8979166676226,0.935950539335165));
#9214=CARTESIAN_POINT('Ctrl Pts',(0.810556943750001,29.8395833342893,1.40392580900275));
#9215=CARTESIAN_POINT('Ctrl Pts',(3.43862649647115E-16,29.7812500009559,
1.87190107867033));
#9216=CARTESIAN_POINT('Ctrl Pts',(-0.810556943749999,29.7229166676226,1.40392580900275));
#9217=CARTESIAN_POINT('Ctrl Pts',(-1.6211138875,29.6645833342893,0.935950539335167));
#9218=CARTESIAN_POINT('Ctrl Pts',(-1.6211138875,29.6062500009559,0.));
#9219=CARTESIAN_POINT('Ctrl Pts',(-1.6211138875,29.5479166676226,-0.935950539335166));
#9220=CARTESIAN_POINT('Ctrl Pts',(-0.81055694375,29.4895833342893,-1.40392580900275));
#9221=CARTESIAN_POINT('Ctrl Pts',(-1.14620883215705E-16,29.4312500009559,
-1.87190107867033));
#9222=CARTESIAN_POINT('Ctrl Pts',(0.81055694375,29.3729166676226,-1.40392580900275));
#9223=CARTESIAN_POINT('Ctrl Pts',(1.6211138875,29.3145833342893,-0.935950539335166));
#9224=CARTESIAN_POINT('Ctrl Pts',(1.6211138875,29.2562500009559,-1.9852919333802E-16));
#9225=CARTESIAN_POINT('Ctrl Pts',(1.6211138875,29.1979166676226,0.935950539335165));
#9226=CARTESIAN_POINT('Ctrl Pts',(0.810556943750001,29.1395833342893,1.40392580900275));
#9227=CARTESIAN_POINT('Ctrl Pts',(3.43862649647115E-16,29.0812500009559,
1.87190107867033));
#9228=CARTESIAN_POINT('Ctrl Pts',(-0.810556943749999,29.0229166676226,1.40392580900275));
#9229=CARTESIAN_POINT('Ctrl Pts',(-1.6211138875,28.9645833342893,0.935950539335167));
#9230=CARTESIAN_POINT('Ctrl Pts',(-1.6211138875,28.9062500009559,0.));
#9231=CARTESIAN_POINT('Ctrl Pts',(-1.6211138875,28.8479166676226,-0.935950539335166));
#9232=CARTESIAN_POINT('Ctrl Pts',(-0.81055694375,28.7895833342893,-1.40392580900275));
#9233=CARTESIAN_POINT('Ctrl Pts',(-1.14620883215705E-16,28.7312500009559,
-1.87190107867033));
#9234=CARTESIAN_POINT('Ctrl Pts',(0.81055694375,28.6729166676226,-1.40392580900275));
#9235=CARTESIAN_POINT('Ctrl Pts',(1.6211138875,28.6145833342893,-0.935950539335166));
#9236=CARTESIAN_POINT('Ctrl Pts',(1.6211138875,28.5562500009559,-1.9852919333802E-16));
#9237=CARTESIAN_POINT('Ctrl Pts',(1.6211138875,28.4979166676226,0.935950539335165));
#9238=CARTESIAN_POINT('Ctrl Pts',(0.810556943750001,28.4395833342893,1.40392580900275));
#9239=CARTESIAN_POINT('Ctrl Pts',(3.43862649647115E-16,28.3812500009559,
1.87190107867033));
#9240=CARTESIAN_POINT('Ctrl Pts',(-0.810556943749999,28.3229166676226,1.40392580900275));
#9241=CARTESIAN_POINT('Ctrl Pts',(-1.6211138875,28.2645833342893,0.935950539335167));
#9242=CARTESIAN_POINT('Ctrl Pts',(-1.6211138875,28.2062500009559,0.));
#9243=CARTESIAN_POINT('Ctrl Pts',(-1.6211138875,28.1479166676226,-0.935950539335166));
#9244=CARTESIAN_POINT('Ctrl Pts',(-0.81055694375,28.0895833342893,-1.40392580900275));
#9245=CARTESIAN_POINT('Ctrl Pts',(-1.14620883215705E-16,28.0312500009559,
-1.87190107867033));
#9246=CARTESIAN_POINT('Ctrl Pts',(0.81055694375,27.9729166676226,-1.40392580900275));
#9247=CARTESIAN_POINT('Ctrl Pts',(1.6211138875,27.9145833342893,-0.935950539335166));
#9248=CARTESIAN_POINT('Ctrl Pts',(1.6211138875,27.8562500009559,-1.9852919333802E-16));
#9249=CARTESIAN_POINT('Ctrl Pts',(1.6211138875,27.7979166676226,0.935950539335165));
#9250=CARTESIAN_POINT('Ctrl Pts',(0.810556943750001,27.7395833342893,1.40392580900275));
#9251=CARTESIAN_POINT('Ctrl Pts',(3.43862649647115E-16,27.6812500009559,
1.87190107867033));
#9252=CARTESIAN_POINT('Ctrl Pts',(-0.810556943749999,27.6229166676226,1.40392580900275));
#9253=CARTESIAN_POINT('Ctrl Pts',(-1.6211138875,27.5645833342893,0.935950539335167));
#9254=CARTESIAN_POINT('Ctrl Pts',(-1.6211138875,27.5062500009559,0.));
#9255=CARTESIAN_POINT('Ctrl Pts',(-1.6211138875,27.4479166676226,-0.935950539335166));
#9256=CARTESIAN_POINT('Ctrl Pts',(-0.81055694375,27.3895833342893,-1.40392580900275));
#9257=CARTESIAN_POINT('Ctrl Pts',(-1.14620883215705E-16,27.3312500009559,
-1.87190107867033));
#9258=CARTESIAN_POINT('Ctrl Pts',(0.81055694375,27.2729166676226,-1.40392580900275));
#9259=CARTESIAN_POINT('Ctrl Pts',(1.6211138875,27.2145833342893,-0.935950539335166));
#9260=CARTESIAN_POINT('Ctrl Pts',(1.6211138875,27.1562500009559,-1.9852919333802E-16));
#9261=CARTESIAN_POINT('Ctrl Pts',(1.6211138875,27.0979166676226,0.935950539335165));
#9262=CARTESIAN_POINT('Ctrl Pts',(0.810556943750001,27.0395833342893,1.40392580900275));
#9263=CARTESIAN_POINT('Ctrl Pts',(3.43862649647115E-16,26.9812500009559,
1.87190107867033));
#9264=CARTESIAN_POINT('Ctrl Pts',(-0.810556943749999,26.9229166676226,1.40392580900275));
#9265=CARTESIAN_POINT('Ctrl Pts',(-1.6211138875,26.8645833342893,0.935950539335167));
#9266=CARTESIAN_POINT('Ctrl Pts',(-1.6211138875,26.8062500009559,0.));
#9267=CARTESIAN_POINT('Ctrl Pts',(-1.6211138875,26.7479166676226,-0.935950539335166));
#9268=CARTESIAN_POINT('Ctrl Pts',(-0.81055694375,26.6895833342893,-1.40392580900275));
#9269=CARTESIAN_POINT('Ctrl Pts',(-1.14620883215705E-16,26.6312500009559,
-1.87190107867033));
#9270=CARTESIAN_POINT('Ctrl Pts',(0.81055694375,26.5729166676226,-1.40392580900275));
#9271=CARTESIAN_POINT('Ctrl Pts',(1.6211138875,26.5145833342893,-0.935950539335166));
#9272=CARTESIAN_POINT('Ctrl Pts',(1.6211138875,26.4562500009559,-1.9852919333802E-16));
#9273=CARTESIAN_POINT('Ctrl Pts',(1.6211138875,26.3979166676226,0.935950539335165));
#9274=CARTESIAN_POINT('Ctrl Pts',(0.810556943750001,26.3395833342893,1.40392580900275));
#9275=CARTESIAN_POINT('Ctrl Pts',(3.43862649647115E-16,26.2812500009559,
1.87190107867033));
#9276=CARTESIAN_POINT('Ctrl Pts',(-0.810556943749999,26.2229166676226,1.40392580900275));
#9277=CARTESIAN_POINT('Ctrl Pts',(-1.6211138875,26.1645833342893,0.935950539335167));
#9278=CARTESIAN_POINT('Ctrl Pts',(-1.6211138875,26.1062500009559,0.));
#9279=CARTESIAN_POINT('Ctrl Pts',(-1.6211138875,26.0479166676226,-0.935950539335166));
#9280=CARTESIAN_POINT('Ctrl Pts',(-0.81055694375,25.9895833342893,-1.40392580900275));
#9281=CARTESIAN_POINT('Ctrl Pts',(-1.14620883215705E-16,25.9312500009559,
-1.87190107867033));
#9282=CARTESIAN_POINT('Ctrl Pts',(0.81055694375,25.8729166676226,-1.40392580900275));
#9283=CARTESIAN_POINT('Ctrl Pts',(1.6211138875,25.8145833342893,-0.935950539335166));
#9284=CARTESIAN_POINT('Ctrl Pts',(1.6211138875,25.7562500009559,-1.9852919333802E-16));
#9285=CARTESIAN_POINT('Ctrl Pts',(1.6211138875,25.6979166676226,0.935950539335165));
#9286=CARTESIAN_POINT('Ctrl Pts',(0.810556943750001,25.6395833342893,1.40392580900275));
#9287=CARTESIAN_POINT('Ctrl Pts',(3.43862649647115E-16,25.5812500009559,
1.87190107867033));
#9288=CARTESIAN_POINT('Ctrl Pts',(-0.810556943749999,25.5229166676226,1.40392580900275));
#9289=CARTESIAN_POINT('Ctrl Pts',(-1.6211138875,25.4645833342893,0.935950539335167));
#9290=CARTESIAN_POINT('Ctrl Pts',(-1.6211138875,25.4062500009559,0.));
#9291=CARTESIAN_POINT('Ctrl Pts',(-1.6211138875,25.3479166676226,-0.935950539335166));
#9292=CARTESIAN_POINT('Ctrl Pts',(-0.81055694375,25.2895833342893,-1.40392580900275));
#9293=CARTESIAN_POINT('Ctrl Pts',(-1.14620883215705E-16,25.2312500009559,
-1.87190107867033));
#9294=CARTESIAN_POINT('Ctrl Pts',(0.81055694375,25.1729166676226,-1.40392580900275));
#9295=CARTESIAN_POINT('Ctrl Pts',(1.6211138875,25.1145833342893,-0.935950539335166));
#9296=CARTESIAN_POINT('Ctrl Pts',(1.6211138875,25.0562500009559,-1.9852919333802E-16));
#9297=CARTESIAN_POINT('Ctrl Pts',(1.6211138875,24.9979166676226,0.935950539335165));
#9298=CARTESIAN_POINT('Ctrl Pts',(0.810556943750001,24.9395833342893,1.40392580900275));
#9299=CARTESIAN_POINT('Ctrl Pts',(3.43862649647115E-16,24.8812500009559,
1.87190107867033));
#9300=CARTESIAN_POINT('Ctrl Pts',(-0.810556943749999,24.8229166676226,1.40392580900275));
#9301=CARTESIAN_POINT('Ctrl Pts',(-1.6211138875,24.7645833342893,0.935950539335167));
#9302=CARTESIAN_POINT('Ctrl Pts',(-1.6211138875,24.7062500009559,0.));
#9303=CARTESIAN_POINT('Ctrl Pts',(-1.6211138875,24.6479166676226,-0.935950539335166));
#9304=CARTESIAN_POINT('Ctrl Pts',(-0.81055694375,24.5895833342893,-1.40392580900275));
#9305=CARTESIAN_POINT('Ctrl Pts',(-1.14620883215705E-16,24.5312500009559,
-1.87190107867033));
#9306=CARTESIAN_POINT('Ctrl Pts',(0.81055694375,24.4729166676226,-1.40392580900275));
#9307=CARTESIAN_POINT('Ctrl Pts',(1.6211138875,24.4145833342893,-0.935950539335166));
#9308=CARTESIAN_POINT('Ctrl Pts',(1.6211138875,24.3562500009559,-1.9852919333802E-16));
#9309=CARTESIAN_POINT('Ctrl Pts',(1.6211138875,24.2979166676226,0.935950539335165));
#9310=CARTESIAN_POINT('Ctrl Pts',(0.810556943750001,24.2395833342893,1.40392580900275));
#9311=CARTESIAN_POINT('Ctrl Pts',(3.43862649647115E-16,24.1812500009559,
1.87190107867033));
#9312=CARTESIAN_POINT('Ctrl Pts',(-0.810556943749999,24.1229166676226,1.40392580900275));
#9313=CARTESIAN_POINT('Ctrl Pts',(-1.6211138875,24.0645833342893,0.935950539335167));
#9314=CARTESIAN_POINT('Ctrl Pts',(-1.6211138875,24.0062500009559,0.));
#9315=CARTESIAN_POINT('Ctrl Pts',(-1.6211138875,23.9479166676226,-0.935950539335166));
#9316=CARTESIAN_POINT('Ctrl Pts',(-0.81055694375,23.8895833342893,-1.40392580900275));
#9317=CARTESIAN_POINT('Ctrl Pts',(-1.14620883215705E-16,23.8312500009559,
-1.87190107867033));
#9318=CARTESIAN_POINT('Ctrl Pts',(0.81055694375,23.7729166676226,-1.40392580900275));
#9319=CARTESIAN_POINT('Ctrl Pts',(1.6211138875,23.7145833342893,-0.935950539335166));
#9320=CARTESIAN_POINT('Ctrl Pts',(1.6211138875,23.6562500009559,-1.9852919333802E-16));
#9321=CARTESIAN_POINT('Ctrl Pts',(1.6211138875,23.5979166676226,0.935950539335165));
#9322=CARTESIAN_POINT('Ctrl Pts',(0.810556943750001,23.5395833342893,1.40392580900275));
#9323=CARTESIAN_POINT('Ctrl Pts',(3.43862649647115E-16,23.4812500009559,
1.87190107867033));
#9324=CARTESIAN_POINT('Ctrl Pts',(-0.810556943749999,23.4229166676226,1.40392580900275));
#9325=CARTESIAN_POINT('Ctrl Pts',(-1.6211138875,23.3645833342893,0.935950539335167));
#9326=CARTESIAN_POINT('Ctrl Pts',(-1.6211138875,23.3062500009559,0.));
#9327=CARTESIAN_POINT('Ctrl Pts',(-1.6211138875,23.2479166676226,-0.935950539335166));
#9328=CARTESIAN_POINT('Ctrl Pts',(-0.81055694375,23.1895833342893,-1.40392580900275));
#9329=CARTESIAN_POINT('Ctrl Pts',(-1.14620883215705E-16,23.1312500009559,
-1.87190107867033));
#9330=CARTESIAN_POINT('Ctrl Pts',(0.81055694375,23.0729166676226,-1.40392580900275));
#9331=CARTESIAN_POINT('Ctrl Pts',(1.6211138875,23.0145833342893,-0.935950539335166));
#9332=CARTESIAN_POINT('Ctrl Pts',(1.6211138875,22.9562500009559,-1.9852919333802E-16));
#9333=CARTESIAN_POINT('Ctrl Pts',(1.6211138875,22.8979166676226,0.935950539335165));
#9334=CARTESIAN_POINT('Ctrl Pts',(0.810556943750001,22.8395833342893,1.40392580900275));
#9335=CARTESIAN_POINT('Ctrl Pts',(3.43862649647115E-16,22.7812500009559,
1.87190107867033));
#9336=CARTESIAN_POINT('Ctrl Pts',(-0.810556943749999,22.7229166676226,1.40392580900275));
#9337=CARTESIAN_POINT('Ctrl Pts',(-1.6211138875,22.6645833342893,0.935950539335167));
#9338=CARTESIAN_POINT('Ctrl Pts',(-1.6211138875,22.6062500009559,0.));
#9339=CARTESIAN_POINT('Ctrl Pts',(-1.6211138875,22.5479166676226,-0.935950539335166));
#9340=CARTESIAN_POINT('Ctrl Pts',(-0.81055694375,22.4895833342893,-1.40392580900275));
#9341=CARTESIAN_POINT('Ctrl Pts',(-1.14620883215705E-16,22.4312500009559,
-1.87190107867033));
#9342=CARTESIAN_POINT('Ctrl Pts',(0.81055694375,22.3729166676226,-1.40392580900275));
#9343=CARTESIAN_POINT('Ctrl Pts',(1.6211138875,22.3145833342893,-0.935950539335166));
#9344=CARTESIAN_POINT('Ctrl Pts',(1.6211138875,22.2562500009559,-1.9852919333802E-16));
#9345=CARTESIAN_POINT('Ctrl Pts',(1.6211138875,22.1979166676226,0.935950539335165));
#9346=CARTESIAN_POINT('Ctrl Pts',(0.810556943750001,22.1395833342893,1.40392580900275));
#9347=CARTESIAN_POINT('Ctrl Pts',(3.43862649647115E-16,22.0812500009559,
1.87190107867033));
#9348=CARTESIAN_POINT('Ctrl Pts',(-0.810556943749999,22.0229166676226,1.40392580900275));
#9349=CARTESIAN_POINT('Ctrl Pts',(-1.6211138875,21.9645833342893,0.935950539335167));
#9350=CARTESIAN_POINT('Ctrl Pts',(-1.6211138875,21.9062500009559,0.));
#9351=CARTESIAN_POINT('Ctrl Pts',(-1.6211138875,21.8479166676226,-0.935950539335166));
#9352=CARTESIAN_POINT('Ctrl Pts',(-0.81055694375,21.7895833342893,-1.40392580900275));
#9353=CARTESIAN_POINT('Ctrl Pts',(-1.14620883215705E-16,21.7312500009559,
-1.87190107867033));
#9354=CARTESIAN_POINT('Ctrl Pts',(0.81055694375,21.6729166676226,-1.40392580900275));
#9355=CARTESIAN_POINT('Ctrl Pts',(1.6211138875,21.6145833342893,-0.935950539335166));
#9356=CARTESIAN_POINT('Ctrl Pts',(1.6211138875,21.5562500009559,-1.9852919333802E-16));
#9357=CARTESIAN_POINT('Ctrl Pts',(1.6211138875,21.4979166676226,0.935950539335165));
#9358=CARTESIAN_POINT('Ctrl Pts',(0.810556943750001,21.4395833342893,1.40392580900275));
#9359=CARTESIAN_POINT('Ctrl Pts',(3.43862649647115E-16,21.3812500009559,
1.87190107867033));
#9360=CARTESIAN_POINT('Ctrl Pts',(-0.810556943749999,21.3229166676226,1.40392580900275));
#9361=CARTESIAN_POINT('Ctrl Pts',(-1.6211138875,21.2645833342893,0.935950539335167));
#9362=CARTESIAN_POINT('Ctrl Pts',(-1.6211138875,21.2062500009559,0.));
#9363=CARTESIAN_POINT('Ctrl Pts',(-1.6211138875,21.1479166676226,-0.935950539335166));
#9364=CARTESIAN_POINT('Ctrl Pts',(-0.81055694375,21.0895833342893,-1.40392580900275));
#9365=CARTESIAN_POINT('Ctrl Pts',(-1.14620883215705E-16,21.0312500009559,
-1.87190107867033));
#9366=CARTESIAN_POINT('Ctrl Pts',(0.81055694375,20.9729166676226,-1.40392580900275));
#9367=CARTESIAN_POINT('Ctrl Pts',(1.6211138875,20.9145833342893,-0.935950539335166));
#9368=CARTESIAN_POINT('Ctrl Pts',(1.6211138875,20.8562500009559,-1.9852919333802E-16));
#9369=CARTESIAN_POINT('Ctrl Pts',(1.6211138875,20.7979166676226,0.935950539335165));
#9370=CARTESIAN_POINT('Ctrl Pts',(0.810556943750001,20.7395833342893,1.40392580900275));
#9371=CARTESIAN_POINT('Ctrl Pts',(3.43862649647115E-16,20.6812500009559,
1.87190107867033));
#9372=CARTESIAN_POINT('Ctrl Pts',(-0.810556943749999,20.6229166676226,1.40392580900275));
#9373=CARTESIAN_POINT('Ctrl Pts',(-1.6211138875,20.5645833342893,0.935950539335167));
#9374=CARTESIAN_POINT('Ctrl Pts',(-1.6211138875,20.5062500009559,0.));
#9375=CARTESIAN_POINT('Ctrl Pts',(-1.6211138875,20.4479166676226,-0.935950539335166));
#9376=CARTESIAN_POINT('Ctrl Pts',(-0.81055694375,20.3895833342893,-1.40392580900275));
#9377=CARTESIAN_POINT('Ctrl Pts',(-1.14620883215705E-16,20.3312500009559,
-1.87190107867033));
#9378=CARTESIAN_POINT('Ctrl Pts',(0.81055694375,20.2729166676226,-1.40392580900275));
#9379=CARTESIAN_POINT('Ctrl Pts',(1.6211138875,20.2145833342893,-0.935950539335166));
#9380=CARTESIAN_POINT('Ctrl Pts',(1.6211138875,20.1562500009559,-1.9852919333802E-16));
#9381=CARTESIAN_POINT('Ctrl Pts',(1.6211138875,20.0979166676226,0.935950539335165));
#9382=CARTESIAN_POINT('Ctrl Pts',(0.810556943750001,20.0395833342893,1.40392580900275));
#9383=CARTESIAN_POINT('Ctrl Pts',(3.43862649647115E-16,19.9812500009559,
1.87190107867033));
#9384=CARTESIAN_POINT('Ctrl Pts',(-0.810556943749999,19.9229166676226,1.40392580900275));
#9385=CARTESIAN_POINT('Ctrl Pts',(-1.6211138875,19.8645833342893,0.935950539335167));
#9386=CARTESIAN_POINT('Ctrl Pts',(-1.6211138875,19.8062500009559,0.));
#9387=CARTESIAN_POINT('Ctrl Pts',(-1.6211138875,19.7479166676226,-0.935950539335166));
#9388=CARTESIAN_POINT('Ctrl Pts',(-0.81055694375,19.6895833342893,-1.40392580900275));
#9389=CARTESIAN_POINT('Ctrl Pts',(-1.14620883215705E-16,19.6312500009559,
-1.87190107867033));
#9390=CARTESIAN_POINT('Ctrl Pts',(0.81055694375,19.5729166676226,-1.40392580900275));
#9391=CARTESIAN_POINT('Ctrl Pts',(1.6211138875,19.5145833342893,-0.935950539335166));
#9392=CARTESIAN_POINT('Ctrl Pts',(1.6211138875,19.4562500009559,-1.9852919333802E-16));
#9393=CARTESIAN_POINT('Ctrl Pts',(1.6211138875,19.3979166676226,0.935950539335165));
#9394=CARTESIAN_POINT('Ctrl Pts',(0.810556943750001,19.3395833342893,1.40392580900275));
#9395=CARTESIAN_POINT('Ctrl Pts',(3.43862649647115E-16,19.2812500009559,
1.87190107867033));
#9396=CARTESIAN_POINT('Ctrl Pts',(-0.810556943749999,19.2229166676226,1.40392580900275));
#9397=CARTESIAN_POINT('Ctrl Pts',(-1.6211138875,19.1645833342893,0.935950539335167));
#9398=CARTESIAN_POINT('Ctrl Pts',(-1.6211138875,19.1062500009559,0.));
#9399=CARTESIAN_POINT('Ctrl Pts',(-1.6211138875,19.0479166676226,-0.935950539335166));
#9400=CARTESIAN_POINT('Ctrl Pts',(-0.81055694375,18.9895833342893,-1.40392580900275));
#9401=CARTESIAN_POINT('Ctrl Pts',(-1.14620883215705E-16,18.9312500009559,
-1.87190107867033));
#9402=CARTESIAN_POINT('Ctrl Pts',(0.81055694375,18.8729166676226,-1.40392580900275));
#9403=CARTESIAN_POINT('Ctrl Pts',(1.6211138875,18.8145833342893,-0.935950539335166));
#9404=CARTESIAN_POINT('Ctrl Pts',(1.6211138875,18.7562500009559,-1.9852919333802E-16));
#9405=CARTESIAN_POINT('Ctrl Pts',(1.6211138875,18.6979166676226,0.935950539335165));
#9406=CARTESIAN_POINT('Ctrl Pts',(0.810556943750001,18.6395833342893,1.40392580900275));
#9407=CARTESIAN_POINT('Ctrl Pts',(3.43862649647115E-16,18.5812500009559,
1.87190107867033));
#9408=CARTESIAN_POINT('Ctrl Pts',(-0.810556943749999,18.5229166676226,1.40392580900275));
#9409=CARTESIAN_POINT('Ctrl Pts',(-1.6211138875,18.4645833342893,0.935950539335167));
#9410=CARTESIAN_POINT('Ctrl Pts',(-1.6211138875,18.4062500009559,0.));
#9411=CARTESIAN_POINT('Ctrl Pts',(-1.6211138875,18.3479166676226,-0.935950539335166));
#9412=CARTESIAN_POINT('Ctrl Pts',(-0.81055694375,18.2895833342893,-1.40392580900275));
#9413=CARTESIAN_POINT('Ctrl Pts',(-1.14620883215705E-16,18.2312500009559,
-1.87190107867033));
#9414=CARTESIAN_POINT('Ctrl Pts',(0.81055694375,18.1729166676226,-1.40392580900275));
#9415=CARTESIAN_POINT('Ctrl Pts',(1.6211138875,18.1145833342893,-0.935950539335166));
#9416=CARTESIAN_POINT('Ctrl Pts',(1.6211138875,18.0562500009559,-1.9852919333802E-16));
#9417=CARTESIAN_POINT('Ctrl Pts',(1.6211138875,17.9979166676226,0.935950539335165));
#9418=CARTESIAN_POINT('Ctrl Pts',(0.810556943750001,17.9395833342893,1.40392580900275));
#9419=CARTESIAN_POINT('Ctrl Pts',(3.43862649647115E-16,17.8812500009559,
1.87190107867033));
#9420=CARTESIAN_POINT('Ctrl Pts',(-0.810556943749999,17.8229166676226,1.40392580900275));
#9421=CARTESIAN_POINT('Ctrl Pts',(-1.6211138875,17.7645833342893,0.935950539335167));
#9422=CARTESIAN_POINT('Ctrl Pts',(-1.6211138875,17.7062500009559,0.));
#9423=CARTESIAN_POINT('Ctrl Pts',(-1.6211138875,17.6479166676226,-0.935950539335166));
#9424=CARTESIAN_POINT('Ctrl Pts',(-0.81055694375,17.5895833342893,-1.40392580900275));
#9425=CARTESIAN_POINT('Ctrl Pts',(-1.14620883215705E-16,17.5312500009559,
-1.87190107867033));
#9426=CARTESIAN_POINT('Ctrl Pts',(0.81055694375,17.4729166676226,-1.40392580900275));
#9427=CARTESIAN_POINT('Ctrl Pts',(1.6211138875,17.4145833342893,-0.935950539335166));
#9428=CARTESIAN_POINT('Ctrl Pts',(1.6211138875,17.3562500009559,-1.9852919333802E-16));
#9429=CARTESIAN_POINT('Ctrl Pts',(1.6211138875,17.2979166676226,0.935950539335165));
#9430=CARTESIAN_POINT('Ctrl Pts',(0.810556943750001,17.2395833342893,1.40392580900275));
#9431=CARTESIAN_POINT('Ctrl Pts',(3.43862649647115E-16,17.1812500009559,
1.87190107867033));
#9432=CARTESIAN_POINT('Ctrl Pts',(-0.810556943749999,17.1229166676226,1.40392580900275));
#9433=CARTESIAN_POINT('Ctrl Pts',(-1.6211138875,17.0645833342893,0.935950539335167));
#9434=CARTESIAN_POINT('Ctrl Pts',(-1.6211138875,17.0062500009559,0.));
#9435=CARTESIAN_POINT('Ctrl Pts',(-1.6211138875,16.9479166676226,-0.935950539335166));
#9436=CARTESIAN_POINT('Ctrl Pts',(-0.81055694375,16.8895833342893,-1.40392580900275));
#9437=CARTESIAN_POINT('Ctrl Pts',(-1.14620883215705E-16,16.8312500009559,
-1.87190107867033));
#9438=CARTESIAN_POINT('Ctrl Pts',(0.81055694375,16.7729166676226,-1.40392580900275));
#9439=CARTESIAN_POINT('Ctrl Pts',(1.6211138875,16.7145833342893,-0.935950539335166));
#9440=CARTESIAN_POINT('Ctrl Pts',(1.6211138875,16.6562500009559,-1.9852919333802E-16));
#9441=CARTESIAN_POINT('Ctrl Pts',(1.6211138875,16.5979166676226,0.935950539335165));
#9442=CARTESIAN_POINT('Ctrl Pts',(0.810556943750001,16.5395833342893,1.40392580900275));
#9443=CARTESIAN_POINT('Ctrl Pts',(3.43862649647115E-16,16.4812500009559,
1.87190107867033));
#9444=CARTESIAN_POINT('Ctrl Pts',(-0.810556943749999,16.4229166676226,1.40392580900275));
#9445=CARTESIAN_POINT('Ctrl Pts',(-1.6211138875,16.3645833342893,0.935950539335167));
#9446=CARTESIAN_POINT('Ctrl Pts',(-1.6211138875,16.3062500009559,0.));
#9447=CARTESIAN_POINT('Ctrl Pts',(-1.6211138875,16.2479166676226,-0.935950539335166));
#9448=CARTESIAN_POINT('Ctrl Pts',(-0.81055694375,16.1895833342893,-1.40392580900275));
#9449=CARTESIAN_POINT('Ctrl Pts',(-1.14620883215705E-16,16.1312500009559,
-1.87190107867033));
#9450=CARTESIAN_POINT('Ctrl Pts',(0.81055694375,16.0729166676226,-1.40392580900275));
#9451=CARTESIAN_POINT('Ctrl Pts',(1.6211138875,16.0145833342893,-0.935950539335166));
#9452=CARTESIAN_POINT('Ctrl Pts',(1.6211138875,15.9562500009559,-1.9852919333802E-16));
#9453=CARTESIAN_POINT('Ctrl Pts',(1.6211138875,15.8979166676226,0.935950539335165));
#9454=CARTESIAN_POINT('Ctrl Pts',(0.810556943750001,15.8395833342893,1.40392580900275));
#9455=CARTESIAN_POINT('Ctrl Pts',(3.43862649647115E-16,15.7812500009559,
1.87190107867033));
#9456=CARTESIAN_POINT('Ctrl Pts',(-0.810556943749999,15.7229166676226,1.40392580900275));
#9457=CARTESIAN_POINT('Ctrl Pts',(-1.6211138875,15.6645833342893,0.935950539335167));
#9458=CARTESIAN_POINT('Ctrl Pts',(-1.6211138875,15.6062500009559,0.));
#9459=CARTESIAN_POINT('Ctrl Pts',(-1.6211138875,15.5479166676226,-0.935950539335166));
#9460=CARTESIAN_POINT('Ctrl Pts',(-0.81055694375,15.4895833342893,-1.40392580900275));
#9461=CARTESIAN_POINT('Ctrl Pts',(-1.14620883215705E-16,15.4312500009559,
-1.87190107867033));
#9462=CARTESIAN_POINT('Ctrl Pts',(0.81055694375,15.3729166676226,-1.40392580900275));
#9463=CARTESIAN_POINT('Ctrl Pts',(1.6211138875,15.3145833342893,-0.935950539335166));
#9464=CARTESIAN_POINT('Ctrl Pts',(1.6211138875,15.2562500009559,-1.9852919333802E-16));
#9465=CARTESIAN_POINT('Ctrl Pts',(1.6211138875,15.1979166676226,0.935950539335165));
#9466=CARTESIAN_POINT('Ctrl Pts',(0.810556943750001,15.1395833342893,1.40392580900275));
#9467=CARTESIAN_POINT('Ctrl Pts',(3.43862649647115E-16,15.0812500009559,
1.87190107867033));
#9468=CARTESIAN_POINT('Ctrl Pts',(-0.810556943749999,15.0229166676226,1.40392580900275));
#9469=CARTESIAN_POINT('Ctrl Pts',(-1.6211138875,14.9645833342893,0.935950539335167));
#9470=CARTESIAN_POINT('Ctrl Pts',(-1.6211138875,14.9062500009559,0.));
#9471=CARTESIAN_POINT('Ctrl Pts',(-1.6211138875,14.8479166676226,-0.935950539335166));
#9472=CARTESIAN_POINT('Ctrl Pts',(-0.81055694375,14.7895833342893,-1.40392580900275));
#9473=CARTESIAN_POINT('Ctrl Pts',(-1.14620883215705E-16,14.7312500009559,
-1.87190107867033));
#9474=CARTESIAN_POINT('Ctrl Pts',(0.81055694375,14.6729166676226,-1.40392580900275));
#9475=CARTESIAN_POINT('Ctrl Pts',(1.6211138875,14.6145833342893,-0.935950539335166));
#9476=CARTESIAN_POINT('Ctrl Pts',(1.6211138875,14.5562500009559,-1.9852919333802E-16));
#9477=CARTESIAN_POINT('Ctrl Pts',(1.6211138875,14.4979166676226,0.935950539335165));
#9478=CARTESIAN_POINT('Ctrl Pts',(0.810556943750001,14.4395833342893,1.40392580900275));
#9479=CARTESIAN_POINT('Ctrl Pts',(3.43862649647115E-16,14.3812500009559,
1.87190107867033));
#9480=CARTESIAN_POINT('Ctrl Pts',(-0.810556943749999,14.3229166676226,1.40392580900275));
#9481=CARTESIAN_POINT('Ctrl Pts',(-1.6211138875,14.2645833342893,0.935950539335167));
#9482=CARTESIAN_POINT('Ctrl Pts',(-1.6211138875,14.2062500009559,0.));
#9483=CARTESIAN_POINT('Ctrl Pts',(-1.6211138875,14.1479166676226,-0.935950539335166));
#9484=CARTESIAN_POINT('Ctrl Pts',(-0.81055694375,14.0895833342893,-1.40392580900275));
#9485=CARTESIAN_POINT('Ctrl Pts',(-1.14620883215705E-16,14.0312500009559,
-1.87190107867033));
#9486=CARTESIAN_POINT('Ctrl Pts',(0.81055694375,13.9729166676226,-1.40392580900275));
#9487=CARTESIAN_POINT('Ctrl Pts',(1.6211138875,13.9145833342893,-0.935950539335166));
#9488=CARTESIAN_POINT('Ctrl Pts',(1.6211138875,13.8562500009559,-1.9852919333802E-16));
#9489=CARTESIAN_POINT('Ctrl Pts',(1.6211138875,13.7979166676226,0.935950539335165));
#9490=CARTESIAN_POINT('Ctrl Pts',(0.810556943750001,13.7395833342893,1.40392580900275));
#9491=CARTESIAN_POINT('Ctrl Pts',(3.43862649647115E-16,13.6812500009559,
1.87190107867033));
#9492=CARTESIAN_POINT('Ctrl Pts',(-0.810556943749999,13.6229166676226,1.40392580900275));
#9493=CARTESIAN_POINT('Ctrl Pts',(-1.6211138875,13.5645833342893,0.935950539335167));
#9494=CARTESIAN_POINT('Ctrl Pts',(-1.6211138875,13.5062500009559,0.));
#9495=CARTESIAN_POINT('Ctrl Pts',(-1.6211138875,13.4479166676226,-0.935950539335166));
#9496=CARTESIAN_POINT('Ctrl Pts',(-0.81055694375,13.3895833342893,-1.40392580900275));
#9497=CARTESIAN_POINT('Ctrl Pts',(-1.14620883215705E-16,13.3312500009559,
-1.87190107867033));
#9498=CARTESIAN_POINT('Ctrl Pts',(0.81055694375,13.2729166676226,-1.40392580900275));
#9499=CARTESIAN_POINT('Ctrl Pts',(1.6211138875,13.2145833342893,-0.935950539335166));
#9500=CARTESIAN_POINT('Ctrl Pts',(1.6211138875,13.1562500009559,-1.9852919333802E-16));
#9501=CARTESIAN_POINT('Ctrl Pts',(1.6211138875,13.0979166676226,0.935950539335165));
#9502=CARTESIAN_POINT('Ctrl Pts',(0.810556943750001,13.0395833342893,1.40392580900275));
#9503=CARTESIAN_POINT('Ctrl Pts',(3.43862649647115E-16,12.9812500009559,
1.87190107867033));
#9504=CARTESIAN_POINT('Ctrl Pts',(-0.810556943749999,12.9229166676226,1.40392580900275));
#9505=CARTESIAN_POINT('Ctrl Pts',(-1.6211138875,12.8645833342893,0.935950539335167));
#9506=CARTESIAN_POINT('Ctrl Pts',(-1.6211138875,12.8062500009559,0.));
#9507=CARTESIAN_POINT('Ctrl Pts',(-1.6211138875,12.7479166676226,-0.935950539335166));
#9508=CARTESIAN_POINT('Ctrl Pts',(-0.81055694375,12.6895833342893,-1.40392580900275));
#9509=CARTESIAN_POINT('Ctrl Pts',(-1.14620883215705E-16,12.6312500009559,
-1.87190107867033));
#9510=CARTESIAN_POINT('Ctrl Pts',(0.81055694375,12.5729166676226,-1.40392580900275));
#9511=CARTESIAN_POINT('Ctrl Pts',(1.6211138875,12.5145833342893,-0.935950539335166));
#9512=CARTESIAN_POINT('Ctrl Pts',(1.6211138875,12.4562500009559,-1.9852919333802E-16));
#9513=CARTESIAN_POINT('Ctrl Pts',(1.6211138875,12.3979166676226,0.935950539335165));
#9514=CARTESIAN_POINT('Ctrl Pts',(0.810556943750001,12.3395833342893,1.40392580900275));
#9515=CARTESIAN_POINT('Ctrl Pts',(3.43862649647115E-16,12.2812500009559,
1.87190107867033));
#9516=CARTESIAN_POINT('Ctrl Pts',(-0.810556943749999,12.2229166676226,1.40392580900275));
#9517=CARTESIAN_POINT('Ctrl Pts',(-1.6211138875,12.1645833342893,0.935950539335167));
#9518=CARTESIAN_POINT('Ctrl Pts',(-1.6211138875,12.1062500009559,0.));
#9519=CARTESIAN_POINT('Ctrl Pts',(-1.6211138875,12.0479166676226,-0.935950539335166));
#9520=CARTESIAN_POINT('Ctrl Pts',(-0.81055694375,11.9895833342893,-1.40392580900275));
#9521=CARTESIAN_POINT('Ctrl Pts',(-1.14620883215705E-16,11.9312500009559,
-1.87190107867033));
#9522=CARTESIAN_POINT('Ctrl Pts',(0.81055694375,11.8729166676226,-1.40392580900275));
#9523=CARTESIAN_POINT('Ctrl Pts',(1.6211138875,11.8145833342893,-0.935950539335166));
#9524=CARTESIAN_POINT('Ctrl Pts',(1.6211138875,11.7562500009559,-1.9852919333802E-16));
#9525=CARTESIAN_POINT('Ctrl Pts',(1.6211138875,11.6979166676226,0.935950539335165));
#9526=CARTESIAN_POINT('Ctrl Pts',(0.810556943750001,11.6395833342893,1.40392580900275));
#9527=CARTESIAN_POINT('Ctrl Pts',(3.43862649647115E-16,11.5812500009559,
1.87190107867033));
#9528=CARTESIAN_POINT('Ctrl Pts',(-0.810556943749999,11.5229166676226,1.40392580900275));
#9529=CARTESIAN_POINT('Ctrl Pts',(-1.6211138875,11.4645833342893,0.935950539335167));
#9530=CARTESIAN_POINT('Ctrl Pts',(-1.6211138875,11.4062500009559,0.));
#9531=CARTESIAN_POINT('Ctrl Pts',(-1.6211138875,11.3479166676226,-0.935950539335166));
#9532=CARTESIAN_POINT('Ctrl Pts',(-0.81055694375,11.2895833342893,-1.40392580900275));
#9533=CARTESIAN_POINT('Ctrl Pts',(-1.14620883215705E-16,11.2312500009559,
-1.87190107867033));
#9534=CARTESIAN_POINT('Ctrl Pts',(0.81055694375,11.1729166676226,-1.40392580900275));
#9535=CARTESIAN_POINT('Ctrl Pts',(1.6211138875,11.1145833342893,-0.935950539335166));
#9536=CARTESIAN_POINT('Ctrl Pts',(1.6211138875,11.0562500009559,-1.9852919333802E-16));
#9537=CARTESIAN_POINT('Ctrl Pts',(1.6211138875,10.9979166676226,0.935950539335165));
#9538=CARTESIAN_POINT('Ctrl Pts',(0.810556943750001,10.9395833342893,1.40392580900275));
#9539=CARTESIAN_POINT('Ctrl Pts',(3.43862649647115E-16,10.8812500009559,
1.87190107867033));
#9540=CARTESIAN_POINT('Ctrl Pts',(-0.810556943749999,10.8229166676226,1.40392580900275));
#9541=CARTESIAN_POINT('Ctrl Pts',(-1.6211138875,10.7645833342893,0.935950539335167));
#9542=CARTESIAN_POINT('Ctrl Pts',(-1.6211138875,10.7062500009559,0.));
#9543=CARTESIAN_POINT('Ctrl Pts',(-1.6211138875,10.6479166676226,-0.935950539335166));
#9544=CARTESIAN_POINT('Ctrl Pts',(-0.81055694375,10.5895833342893,-1.40392580900275));
#9545=CARTESIAN_POINT('Ctrl Pts',(-1.14620883215705E-16,10.5312500009559,
-1.87190107867033));
#9546=CARTESIAN_POINT('Ctrl Pts',(0.81055694375,10.4729166676226,-1.40392580900275));
#9547=CARTESIAN_POINT('Ctrl Pts',(1.6211138875,10.4145833342893,-0.935950539335166));
#9548=CARTESIAN_POINT('Ctrl Pts',(1.6211138875,10.3562500009559,-1.9852919333802E-16));
#9549=CARTESIAN_POINT('Ctrl Pts',(1.6211138875,10.2979166676226,0.935950539335165));
#9550=CARTESIAN_POINT('Ctrl Pts',(0.810556943750001,10.2395833342893,1.40392580900275));
#9551=CARTESIAN_POINT('Ctrl Pts',(3.43862649647115E-16,10.1812500009559,
1.87190107867033));
#9552=CARTESIAN_POINT('Ctrl Pts',(-0.810556943749999,10.1229166676226,1.40392580900275));
#9553=CARTESIAN_POINT('Ctrl Pts',(-1.6211138875,10.0645833342893,0.935950539335167));
#9554=CARTESIAN_POINT('Ctrl Pts',(-1.6211138875,10.0062500009559,0.));
#9555=CARTESIAN_POINT('Ctrl Pts',(-1.6211138875,9.94791666762259,-0.935950539335166));
#9556=CARTESIAN_POINT('Ctrl Pts',(-0.81055694375,9.88958333428926,-1.40392580900275));
#9557=CARTESIAN_POINT('Ctrl Pts',(-1.14620883215705E-16,9.83125000095593,
-1.87190107867033));
#9558=CARTESIAN_POINT('Ctrl Pts',(0.81055694375,9.7729166676226,-1.40392580900275));
#9559=CARTESIAN_POINT('Ctrl Pts',(1.6211138875,9.71458333428926,-0.935950539335166));
#9560=CARTESIAN_POINT('Ctrl Pts',(1.6211138875,9.65625000095593,-1.9852919333802E-16));
#9561=CARTESIAN_POINT('Ctrl Pts',(1.6211138875,9.59791666762259,0.935950539335165));
#9562=CARTESIAN_POINT('Ctrl Pts',(0.810556943750001,9.53958333428926,1.40392580900275));
#9563=CARTESIAN_POINT('Ctrl Pts',(3.43862649647115E-16,9.48125000095593,
1.87190107867033));
#9564=CARTESIAN_POINT('Ctrl Pts',(-0.810556943749999,9.42291666762259,1.40392580900275));
#9565=CARTESIAN_POINT('Ctrl Pts',(-1.6211138875,9.36458333428926,0.935950539335167));
#9566=CARTESIAN_POINT('Ctrl Pts',(-1.6211138875,9.30625000095593,0.));
#9567=CARTESIAN_POINT('Ctrl Pts',(-1.6211138875,9.24791666762259,-0.935950539335166));
#9568=CARTESIAN_POINT('Ctrl Pts',(-0.81055694375,9.18958333428926,-1.40392580900275));
#9569=CARTESIAN_POINT('Ctrl Pts',(-1.14620883215705E-16,9.13125000095592,
-1.87190107867033));
#9570=CARTESIAN_POINT('Ctrl Pts',(0.81055694375,9.0729166676226,-1.40392580900275));
#9571=CARTESIAN_POINT('Ctrl Pts',(1.6211138875,9.01458333428926,-0.935950539335166));
#9572=CARTESIAN_POINT('Ctrl Pts',(1.6211138875,8.95625000095593,-1.9852919333802E-16));
#9573=CARTESIAN_POINT('Ctrl Pts',(1.6211138875,8.89791666762259,0.935950539335165));
#9574=CARTESIAN_POINT('Ctrl Pts',(0.810556943750001,8.83958333428926,1.40392580900275));
#9575=CARTESIAN_POINT('Ctrl Pts',(3.43862649647115E-16,8.78125000095592,
1.87190107867033));
#9576=CARTESIAN_POINT('Ctrl Pts',(-0.810556943749999,8.72291666762259,1.40392580900275));
#9577=CARTESIAN_POINT('Ctrl Pts',(-1.6211138875,8.66458333428927,0.935950539335167));
#9578=CARTESIAN_POINT('Ctrl Pts',(-1.6211138875,8.60625000095593,0.));
#9579=CARTESIAN_POINT('Ctrl Pts',(-1.6211138875,8.5479166676226,-0.935950539335166));
#9580=CARTESIAN_POINT('Ctrl Pts',(-0.81055694375,8.48958333428926,-1.40392580900275));
#9581=CARTESIAN_POINT('Ctrl Pts',(-1.14620883215705E-16,8.43125000095593,
-1.87190107867033));
#9582=CARTESIAN_POINT('Ctrl Pts',(0.81055694375,8.37291666762259,-1.40392580900275));
#9583=CARTESIAN_POINT('Ctrl Pts',(1.6211138875,8.31458333428926,-0.935950539335166));
#9584=CARTESIAN_POINT('Ctrl Pts',(1.6211138875,8.25625000095592,-1.9852919333802E-16));
#9585=CARTESIAN_POINT('Ctrl Pts',(1.6211138875,8.1979166676226,0.935950539335165));
#9586=CARTESIAN_POINT('Ctrl Pts',(0.810556943750001,8.13958333428925,1.40392580900275));
#9587=CARTESIAN_POINT('Ctrl Pts',(3.43862649647115E-16,8.08125000095593,
1.87190107867033));
#9588=CARTESIAN_POINT('Ctrl Pts',(-0.810556943749999,8.02291666762259,1.40392580900275));
#9589=CARTESIAN_POINT('Ctrl Pts',(-1.6211138875,7.96458333428926,0.935950539335167));
#9590=CARTESIAN_POINT('Ctrl Pts',(-1.6211138875,7.90625000095593,0.));
#9591=CARTESIAN_POINT('Ctrl Pts',(-1.6211138875,7.84791666762259,-0.935950539335166));
#9592=CARTESIAN_POINT('Ctrl Pts',(-0.81055694375,7.78958333428927,-1.40392580900275));
#9593=CARTESIAN_POINT('Ctrl Pts',(-1.14620883215705E-16,7.73125000095592,
-1.87190107867033));
#9594=CARTESIAN_POINT('Ctrl Pts',(0.81055694375,7.6729166676226,-1.40392580900275));
#9595=CARTESIAN_POINT('Ctrl Pts',(1.6211138875,7.61458333428926,-0.935950539335166));
#9596=CARTESIAN_POINT('Ctrl Pts',(1.6211138875,7.55625000095593,-1.9852919333802E-16));
#9597=CARTESIAN_POINT('Ctrl Pts',(1.6211138875,7.49791666762259,0.935950539335165));
#9598=CARTESIAN_POINT('Ctrl Pts',(0.810556943750001,7.43958333428926,1.40392580900275));
#9599=CARTESIAN_POINT('Ctrl Pts',(3.43862649647115E-16,7.38125000095592,
1.87190107867033));
#9600=CARTESIAN_POINT('Ctrl Pts',(-0.810556943749999,7.3229166676226,1.40392580900275));
#9601=CARTESIAN_POINT('Ctrl Pts',(-1.6211138875,7.26458333428925,0.935950539335167));
#9602=CARTESIAN_POINT('Ctrl Pts',(-1.6211138875,7.20625000095593,0.));
#9603=CARTESIAN_POINT('Ctrl Pts',(-1.6211138875,7.1479166676226,-0.935950539335166));
#9604=CARTESIAN_POINT('Ctrl Pts',(-0.81055694375,7.08958333428926,-1.40392580900275));
#9605=CARTESIAN_POINT('Ctrl Pts',(-1.14620883215705E-16,7.03125000095593,
-1.87190107867033));
#9606=CARTESIAN_POINT('Ctrl Pts',(0.81055694375,6.97291666762259,-1.40392580900275));
#9607=CARTESIAN_POINT('Ctrl Pts',(1.6211138875,6.91458333428927,-0.935950539335166));
#9608=CARTESIAN_POINT('Ctrl Pts',(1.6211138875,6.85625000095592,-1.9852919333802E-16));
#9609=CARTESIAN_POINT('Ctrl Pts',(1.6211138875,6.7979166676226,0.935950539335165));
#9610=CARTESIAN_POINT('Ctrl Pts',(0.810556943750001,6.73958333428926,1.40392580900275));
#9611=CARTESIAN_POINT('Ctrl Pts',(3.43862649647115E-16,6.68125000095593,
1.87190107867033));
#9612=CARTESIAN_POINT('Ctrl Pts',(-0.810556943749999,6.62291666762259,1.40392580900275));
#9613=CARTESIAN_POINT('Ctrl Pts',(-1.6211138875,6.56458333428926,0.935950539335167));
#9614=CARTESIAN_POINT('Ctrl Pts',(-1.6211138875,6.50625000095592,0.));
#9615=CARTESIAN_POINT('Ctrl Pts',(-1.6211138875,6.44791666762259,-0.935950539335166));
#9616=CARTESIAN_POINT('Ctrl Pts',(-0.81055694375,6.38958333428925,-1.40392580900275));
#9617=CARTESIAN_POINT('Ctrl Pts',(-1.14620883215705E-16,6.33125000095593,
-1.87190107867033));
#9618=CARTESIAN_POINT('Ctrl Pts',(0.81055694375,6.2729166676226,-1.40392580900275));
#9619=CARTESIAN_POINT('Ctrl Pts',(1.6211138875,6.21458333428926,-0.935950539335166));
#9620=CARTESIAN_POINT('Ctrl Pts',(1.6211138875,6.15625000095593,-1.9852919333802E-16));
#9621=CARTESIAN_POINT('Ctrl Pts',(1.6211138875,6.09791666762259,0.935950539335165));
#9622=CARTESIAN_POINT('Ctrl Pts',(0.810556943750001,6.03958333428927,1.40392580900275));
#9623=CARTESIAN_POINT('Ctrl Pts',(3.43862649647115E-16,5.98125000095592,
1.87190107867033));
#9624=CARTESIAN_POINT('Ctrl Pts',(-0.810556943749999,5.9229166676226,1.40392580900275));
#9625=CARTESIAN_POINT('Ctrl Pts',(-1.6211138875,5.86458333428926,0.935950539335167));
#9626=CARTESIAN_POINT('Ctrl Pts',(-1.6211138875,5.80625000095593,0.));
#9627=CARTESIAN_POINT('Ctrl Pts',(-1.6211138875,5.74791666762259,-0.935950539335166));
#9628=CARTESIAN_POINT('Ctrl Pts',(-0.81055694375,5.68958333428926,-1.40392580900275));
#9629=CARTESIAN_POINT('Ctrl Pts',(-1.14620883215705E-16,5.63125000095592,
-1.87190107867033));
#9630=CARTESIAN_POINT('Ctrl Pts',(0.81055694375,5.57291666762259,-1.40392580900275));
#9631=CARTESIAN_POINT('Ctrl Pts',(1.6211138875,5.51458333428927,-0.935950539335166));
#9632=CARTESIAN_POINT('Ctrl Pts',(1.6211138875,5.45625000095593,-1.9852919333802E-16));
#9633=CARTESIAN_POINT('Ctrl Pts',(1.6211138875,5.3979166676226,0.935950539335165));
#9634=CARTESIAN_POINT('Ctrl Pts',(0.810556943750001,5.33958333428926,1.40392580900275));
#9635=CARTESIAN_POINT('Ctrl Pts',(3.43862649647115E-16,5.28125000095593,
1.87190107867033));
#9636=CARTESIAN_POINT('Ctrl Pts',(-0.810556943749999,5.22291666762259,1.40392580900275));
#9637=CARTESIAN_POINT('Ctrl Pts',(-1.6211138875,5.16458333428926,0.935950539335167));
#9638=CARTESIAN_POINT('Ctrl Pts',(-1.6211138875,5.10625000095592,0.));
#9639=CARTESIAN_POINT('Ctrl Pts',(-1.6211138875,5.0479166676226,-0.935950539335166));
#9640=CARTESIAN_POINT('Ctrl Pts',(-0.81055694375,4.98958333428925,-1.40392580900275));
#9641=CARTESIAN_POINT('Ctrl Pts',(-1.14620883215705E-16,4.93125000095593,
-1.87190107867033));
#9642=CARTESIAN_POINT('Ctrl Pts',(0.81055694375,4.87291666762259,-1.40392580900275));
#9643=CARTESIAN_POINT('Ctrl Pts',(1.6211138875,4.81458333428926,-0.935950539335166));
#9644=CARTESIAN_POINT('Ctrl Pts',(1.6211138875,4.75625000095593,-1.9852919333802E-16));
#9645=CARTESIAN_POINT('Ctrl Pts',(1.6211138875,4.69791666762259,0.935950539335165));
#9646=CARTESIAN_POINT('Ctrl Pts',(0.810556943750001,4.63958333428927,1.40392580900275));
#9647=CARTESIAN_POINT('Ctrl Pts',(3.43862649647115E-16,4.58125000095593,
1.87190107867033));
#9648=CARTESIAN_POINT('Ctrl Pts',(-0.810556943749999,4.5229166676226,1.40392580900275));
#9649=CARTESIAN_POINT('Ctrl Pts',(-1.6211138875,4.46458333428926,0.935950539335167));
#9650=CARTESIAN_POINT('Ctrl Pts',(-1.6211138875,4.40625000095593,0.));
#9651=CARTESIAN_POINT('Ctrl Pts',(-1.6211138875,4.34791666762259,-0.935950539335166));
#9652=CARTESIAN_POINT('Ctrl Pts',(-0.81055694375,4.28958333428926,-1.40392580900275));
#9653=CARTESIAN_POINT('Ctrl Pts',(-1.14620883215705E-16,4.23125000095592,
-1.87190107867033));
#9654=CARTESIAN_POINT('Ctrl Pts',(0.81055694375,4.17291666762259,-1.40392580900275));
#9655=CARTESIAN_POINT('Ctrl Pts',(1.6211138875,4.11458333428925,-0.935950539335166));
#9656=CARTESIAN_POINT('Ctrl Pts',(1.6211138875,4.05625000095593,-1.9852919333802E-16));
#9657=CARTESIAN_POINT('Ctrl Pts',(1.6211138875,3.9979166676226,0.935950539335165));
#9658=CARTESIAN_POINT('Ctrl Pts',(0.810556943750001,3.93958333428926,1.40392580900275));
#9659=CARTESIAN_POINT('Ctrl Pts',(3.43862649647115E-16,3.88125000095593,
1.87190107867033));
#9660=CARTESIAN_POINT('Ctrl Pts',(-0.810556943749999,3.82291666762259,1.40392580900275));
#9661=CARTESIAN_POINT('Ctrl Pts',(-1.6211138875,3.76458333428927,0.935950539335167));
#9662=CARTESIAN_POINT('Ctrl Pts',(-1.6211138875,3.70625000095592,0.));
#9663=CARTESIAN_POINT('Ctrl Pts',(-1.6211138875,3.6479166676226,-0.935950539335166));
#9664=CARTESIAN_POINT('Ctrl Pts',(-0.81055694375,3.58958333428926,-1.40392580900275));
#9665=CARTESIAN_POINT('Ctrl Pts',(-1.14620883215705E-16,3.53125000095593,
-1.87190107867033));
#9666=CARTESIAN_POINT('Ctrl Pts',(0.81055694375,3.47291666762259,-1.40392580900275));
#9667=CARTESIAN_POINT('Ctrl Pts',(1.6211138875,3.41458333428926,-0.935950539335166));
#9668=CARTESIAN_POINT('Ctrl Pts',(1.6211138875,3.35625000095592,-1.9852919333802E-16));
#9669=CARTESIAN_POINT('Ctrl Pts',(1.6211138875,3.29791666762259,0.935950539335165));
#9670=CARTESIAN_POINT('Ctrl Pts',(0.810556943750001,3.23958333428925,1.40392580900275));
#9671=CARTESIAN_POINT('Ctrl Pts',(3.43862649647115E-16,3.18125000095593,
1.87190107867033));
#9672=CARTESIAN_POINT('Ctrl Pts',(-0.810556943749999,3.1229166676226,1.40392580900275));
#9673=CARTESIAN_POINT('Ctrl Pts',(-1.6211138875,3.06458333428926,0.935950539335167));
#9674=CARTESIAN_POINT('Ctrl Pts',(-1.6211138875,3.00625000095593,0.));
#9675=CARTESIAN_POINT('Ctrl Pts',(-1.6211138875,2.94791666762259,-0.935950539335166));
#9676=CARTESIAN_POINT('Ctrl Pts',(-0.81055694375,2.88958333428926,-1.40392580900275));
#9677=CARTESIAN_POINT('Ctrl Pts',(-1.14620883215705E-16,2.83125000095592,
-1.87190107867033));
#9678=CARTESIAN_POINT('Ctrl Pts',(0.81055694375,2.7729166676226,-1.40392580900275));
#9679=CARTESIAN_POINT('Ctrl Pts',(1.6211138875,2.71458333428926,-0.935950539335166));
#9680=CARTESIAN_POINT('Ctrl Pts',(1.6211138875,2.65625000095593,-1.9852919333802E-16));
#9681=CARTESIAN_POINT('Ctrl Pts',(1.6211138875,2.59791666762259,0.935950539335165));
#9682=CARTESIAN_POINT('Ctrl Pts',(0.810556943750001,2.53958333428926,1.40392580900275));
#9683=CARTESIAN_POINT('Ctrl Pts',(3.43862649647115E-16,2.48125000095592,
1.87190107867033));
#9684=CARTESIAN_POINT('Ctrl Pts',(-0.810556943749999,2.42291666762259,1.40392580900275));
#9685=CARTESIAN_POINT('Ctrl Pts',(-1.6211138875,2.36458333428927,0.935950539335167));
#9686=CARTESIAN_POINT('Ctrl Pts',(-1.6211138875,2.30625000095593,0.));
#9687=CARTESIAN_POINT('Ctrl Pts',(-1.6211138875,2.2479166676226,-0.935950539335166));
#9688=CARTESIAN_POINT('Ctrl Pts',(-0.81055694375,2.18958333428926,-1.40392580900275));
#9689=CARTESIAN_POINT('Ctrl Pts',(-1.14620883215705E-16,2.13125000095593,
-1.87190107867033));
#9690=CARTESIAN_POINT('Ctrl Pts',(0.81055694375,2.07291666762259,-1.40392580900275));
#9691=CARTESIAN_POINT('Ctrl Pts',(1.6211138875,2.01458333428926,-0.935950539335166));
#9692=CARTESIAN_POINT('Ctrl Pts',(1.6211138875,1.95625000095592,-1.9852919333802E-16));
#9693=CARTESIAN_POINT('Ctrl Pts',(1.6211138875,1.8979166676226,0.935950539335165));
#9694=CARTESIAN_POINT('Ctrl Pts',(0.810556943750001,1.83958333428925,1.40392580900275));
#9695=CARTESIAN_POINT('Ctrl Pts',(3.43862649647115E-16,1.78125000095593,
1.87190107867033));
#9696=CARTESIAN_POINT('Ctrl Pts',(-0.810556943749999,1.72291666762259,1.40392580900275));
#9697=CARTESIAN_POINT('Ctrl Pts',(-1.6211138875,1.66458333428926,0.935950539335167));
#9698=CARTESIAN_POINT('Ctrl Pts',(-1.6211138875,1.60625000095593,0.));
#9699=CARTESIAN_POINT('Ctrl Pts',(-1.6211138875,1.54791666762259,-0.935950539335166));
#9700=CARTESIAN_POINT('Ctrl Pts',(-0.81055694375,1.48958333428927,-1.40392580900275));
#9701=CARTESIAN_POINT('Ctrl Pts',(-1.14620883215705E-16,1.43125000095592,
-1.87190107867033));
#9702=CARTESIAN_POINT('Ctrl Pts',(0.81055694375,1.3729166676226,-1.40392580900275));
#9703=CARTESIAN_POINT('Ctrl Pts',(1.6211138875,1.31458333428926,-0.935950539335166));
#9704=CARTESIAN_POINT('Ctrl Pts',(1.6211138875,1.25625000095593,-1.9852919333802E-16));
#9705=CARTESIAN_POINT('Ctrl Pts',(1.6211138875,1.19791666762259,0.935950539335165));
#9706=CARTESIAN_POINT('Ctrl Pts',(0.810556943750001,1.13958333428926,1.40392580900275));
#9707=CARTESIAN_POINT('Ctrl Pts',(3.43862649647115E-16,1.08125000095592,
1.87190107867033));
#9708=CARTESIAN_POINT('Ctrl Pts',(-0.810556943749999,1.02291666762259,1.40392580900275));
#9709=CARTESIAN_POINT('Ctrl Pts',(-1.6211138875,0.964583334289254,0.935950539335167));
#9710=CARTESIAN_POINT('Ctrl Pts',(-1.6211138875,0.906250000955927,0.));
#9711=CARTESIAN_POINT('Ctrl Pts',(-1.6211138875,0.8479166676226,-0.935950539335166));
#9712=CARTESIAN_POINT('Ctrl Pts',(-0.81055694375,0.789583334289259,-1.40392580900275));
#9713=CARTESIAN_POINT('Ctrl Pts',(-1.14620883215705E-16,0.731250000955933,
-1.87190107867033));
#9714=CARTESIAN_POINT('Ctrl Pts',(0.81055694375,0.672916667622592,-1.40392580900275));
#9715=CARTESIAN_POINT('Ctrl Pts',(1.6211138875,0.614583334289265,-0.935950539335166));
#9716=CARTESIAN_POINT('Ctrl Pts',(1.6211138875,0.556250000955924,-1.9852919333802E-16));
#9717=CARTESIAN_POINT('Ctrl Pts',(1.6211138875,0.497916667622597,0.935950539335165));
#9718=CARTESIAN_POINT('Ctrl Pts',(0.810556943750001,0.439583334289256,1.40392580900275));
#9719=CARTESIAN_POINT('Ctrl Pts',(3.43862649647115E-16,0.381250000955929,
1.87190107867033));
#9720=CARTESIAN_POINT('Ctrl Pts',(-0.810556943749999,0.322916667622589,
1.40392580900275));
#9721=CARTESIAN_POINT('Ctrl Pts',(-1.6211138875,0.264583334289262,0.935950539335167));
#9722=CARTESIAN_POINT('Ctrl Pts',(-1.6211138875,0.206250000955921,0.));
#9723=CARTESIAN_POINT('Ctrl Pts',(-1.6211138875,0.147916667622594,-0.935950539335166));
#9724=CARTESIAN_POINT('Ctrl Pts',(-0.81055694375,0.0895833342892532,-1.40392580900275));
#9725=CARTESIAN_POINT('Ctrl Pts',(-1.14620883215705E-16,0.0312500009559263,
-1.87190107867033));
#9726=CARTESIAN_POINT('Ctrl Pts',(0.81055694375,-0.0270833323774006,-1.40392580900275));
#9727=CARTESIAN_POINT('Ctrl Pts',(1.6211138875,-0.0854166657107414,-0.935950539335166));
#9728=CARTESIAN_POINT('Ctrl Pts',(1.6211138875,-0.143749999044068,-1.9852919333802E-16));
#9729=CARTESIAN_POINT('Ctrl Pts',(1.6211138875,-0.202083332377409,0.935950539335165));
#9730=CARTESIAN_POINT('Ctrl Pts',(0.810556943750001,-0.260416665710736,
1.40392580900275));
#9731=CARTESIAN_POINT('Ctrl Pts',(3.43862649647115E-16,-0.318749999044077,
1.87190107867033));
#9732=CARTESIAN_POINT('Ctrl Pts',(-0.810556943749999,-0.377083332377404,
1.40392580900275));
#9733=CARTESIAN_POINT('Ctrl Pts',(-1.6211138875,-0.435416665710744,0.935950539335167));
#9734=CARTESIAN_POINT('Ctrl Pts',(-1.6211138875,-0.493749999044071,0.));
#9735=CARTESIAN_POINT('Ctrl Pts',(-1.6211138875,-0.552083332377412,-0.935950539335166));
#9736=CARTESIAN_POINT('Ctrl Pts',(-0.81055694375,-0.610416665710739,-1.40392580900275));
#9737=CARTESIAN_POINT('Ctrl Pts',(-1.14620883215705E-16,-0.66874999904408,
-1.87190107867033));
#9738=CARTESIAN_POINT('Ctrl Pts',(0.81055694375,-0.727083332377407,-1.40392580900275));
#9739=CARTESIAN_POINT('Ctrl Pts',(1.6211138875,-0.785416665710734,-0.935950539335166));
#9740=CARTESIAN_POINT('Ctrl Pts',(1.6211138875,-0.843749999044074,-1.9852919333802E-16));
#9741=CARTESIAN_POINT('Ctrl Pts',(1.6211138875,-0.902083332377402,0.935950539335165));
#9742=CARTESIAN_POINT('Ctrl Pts',(0.810556943750001,-0.960416665710742,
1.40392580900275));
#9743=CARTESIAN_POINT('Ctrl Pts',(3.43862649647115E-16,-1.01874999904407,
1.87190107867033));
#9744=CARTESIAN_POINT('Ctrl Pts',(-0.810556943749999,-1.07708333237741,
1.40392580900275));
#9745=CARTESIAN_POINT('Ctrl Pts',(-1.6211138875,-1.13541666571074,0.935950539335167));
#9746=CARTESIAN_POINT('Ctrl Pts',(-1.6211138875,-1.19374999904408,0.));
#9747=CARTESIAN_POINT('Ctrl Pts',(-1.6211138875,-1.2520833323774,-0.935950539335166));
#9748=CARTESIAN_POINT('Ctrl Pts',(-0.81055694375,-1.31041666571075,-1.40392580900275));
#9749=CARTESIAN_POINT('Ctrl Pts',(-1.14620883215705E-16,-1.36874999904407,
-1.87190107867033));
#9750=CARTESIAN_POINT('Ctrl Pts',(0.81055694375,-1.42708333237741,-1.40392580900275));
#9751=CARTESIAN_POINT('Ctrl Pts',(1.6211138875,-1.48541666571074,-0.935950539335166));
#9752=CARTESIAN_POINT('Ctrl Pts',(1.6211138875,-1.54374999904407,-1.9852919333802E-16));
#9753=CARTESIAN_POINT('Ctrl Pts',(1.6211138875,-1.60208333237741,0.935950539335165));
#9754=CARTESIAN_POINT('Ctrl Pts',(0.810556943750001,-1.66041666571073,1.40392580900275));
#9755=CARTESIAN_POINT('Ctrl Pts',(3.43862649647115E-16,-1.71874999904408,
1.87190107867033));
#9756=CARTESIAN_POINT('Ctrl Pts',(-0.810556943749999,-1.7770833323774,1.40392580900275));
#9757=CARTESIAN_POINT('Ctrl Pts',(-1.6211138875,-1.83541666571074,0.935950539335167));
#9758=CARTESIAN_POINT('Ctrl Pts',(-1.6211138875,-1.89374999904407,0.));
#9759=CARTESIAN_POINT('Ctrl Pts',(-1.6211138875,-1.95208333237741,-0.935950539335166));
#9760=CARTESIAN_POINT('Ctrl Pts',(-0.81055694375,-2.01041666571074,-1.40392580900275));
#9761=CARTESIAN_POINT('Ctrl Pts',(-1.14620883215705E-16,-2.06874999904408,
-1.87190107867033));
#9762=CARTESIAN_POINT('Ctrl Pts',(0.81055694375,-2.12708333237741,-1.40392580900275));
#9763=CARTESIAN_POINT('Ctrl Pts',(1.6211138875,-2.18541666571075,-0.935950539335166));
#9764=CARTESIAN_POINT('Ctrl Pts',(1.6211138875,-2.24374999904407,-1.9852919333802E-16));
#9765=CARTESIAN_POINT('Ctrl Pts',(1.6211138875,-2.3020833323774,0.935950539335165));
#9766=CARTESIAN_POINT('Ctrl Pts',(0.810556943750001,-2.36041666571074,1.40392580900275));
#9767=CARTESIAN_POINT('Ctrl Pts',(0.598929625666448,-2.37564684414964,1.52610889806617));
#9768=CARTESIAN_POINT('Ctrl Pts',(0.360688737133008,-2.39279232081431,1.5804790005409));
#9769=CARTESIAN_POINT('Ctrl Pts',(1.48613470695839,9.52000000000001,-1.33843019915343));
#9770=CARTESIAN_POINT('Ctrl Pts',(1.57630516101018,9.52000000000001,-1.2160238520719));
#9771=CARTESIAN_POINT('Ctrl Pts',(1.64972854045747,9.52000000000002,-1.08718013570266));
#9772=CARTESIAN_POINT('Ctrl Pts',(1.76662380592186,9.52000000000001,-0.814456482417219));
#9773=CARTESIAN_POINT('Ctrl Pts',(1.80998962761493,9.52000000000002,-0.669151004255831));
#9774=CARTESIAN_POINT('Ctrl Pts',(1.88756293094029,9.52000000000002,-0.231172020581771));
#9775=CARTESIAN_POINT('Ctrl Pts',(1.87351731814856,9.52000000000001,0.075154658113733));
#9776=CARTESIAN_POINT('Ctrl Pts',(1.74098688976458,9.52,0.499507026686462));
#9777=CARTESIAN_POINT('Ctrl Pts',(1.67755793546182,9.52,0.637636609961961));
#9778=CARTESIAN_POINT('Ctrl Pts',(1.52046925826298,9.51999999999999,0.888986033250457));
#9779=CARTESIAN_POINT('Ctrl Pts',(1.42490873390712,9.52000000000001,1.005753839455));
#9780=CARTESIAN_POINT('Ctrl Pts',(1.20787534958114,9.52000000000001,1.2103878868076));
#9781=CARTESIAN_POINT('Ctrl Pts',(1.08796092139376,9.52000000000001,1.29758441757011));
#9782=CARTESIAN_POINT('Ctrl Pts',(0.825073157518373,9.52000000000001,1.44138701387347));
#9783=CARTESIAN_POINT('Ctrl Pts',(0.68525065841953,9.52000000000001,1.49601523748159));
#9784=CARTESIAN_POINT('Ctrl Pts',(0.538440894222362,9.51999996467551,1.52908195976357));
#9785=CARTESIAN_POINT('Origin',(0.,0.,0.));
#9786=CARTESIAN_POINT('Origin',(0.,9.52000000000001,0.));
#9787=CARTESIAN_POINT('Origin',(0.,12.,0.));
#9788=CARTESIAN_POINT('',(-9.71064220297663E-16,12.,1.61658075373095));
#9789=CARTESIAN_POINT('',(-1.4,12.,0.808290376865476));
#9790=CARTESIAN_POINT('',(-1.325,12.,0.851591647054698));
#9791=CARTESIAN_POINT('',(-1.4,12.,-0.808290376865476));
#9792=CARTESIAN_POINT('',(-1.4,12.,-0.721687836487033));
#9793=CARTESIAN_POINT('',(1.9499918173238E-16,12.,-1.61658075373095));
#9794=CARTESIAN_POINT('',(-0.0749999999999998,12.,-1.57327948354173));
#9795=CARTESIAN_POINT('',(1.4,12.,-0.808290376865477));
#9796=CARTESIAN_POINT('',(1.325,12.,-0.851591647054698));
#9797=CARTESIAN_POINT('',(1.4,12.,0.808290376865476));
#9798=CARTESIAN_POINT('',(1.4,12.,0.721687836487033));
#9799=CARTESIAN_POINT('',(0.0749999999999994,12.,1.57327948354173));
#9800=CARTESIAN_POINT('Origin',(1.25,10.5,-0.721687836487033));
#9801=CARTESIAN_POINT('',(1.24999999999999,10.5,-0.721687836487047));
#9802=CARTESIAN_POINT('',(1.25,11.85,-0.721687836487033));
#9803=CARTESIAN_POINT('',(1.25,10.5,-0.721687836487033));
#9804=CARTESIAN_POINT('',(-1.09387392956801E-17,11.85,-1.44337567297407));
#9805=CARTESIAN_POINT('',(-5.42101086242752E-17,11.85,-1.44337567297407));
#9806=CARTESIAN_POINT('',(-1.09387392956801E-17,10.5,-1.44337567297407));
#9807=CARTESIAN_POINT('',(-1.09387392956801E-17,10.5,-1.44337567297407));
#9808=CARTESIAN_POINT('',(1.25,10.5,-0.721687836487033));
#9809=CARTESIAN_POINT('Origin',(1.25,10.5,0.721687836487033));
#9810=CARTESIAN_POINT('',(1.25,10.5,0.721687836487033));
#9811=CARTESIAN_POINT('',(1.25,11.85,0.721687836487033));
#9812=CARTESIAN_POINT('',(1.25,10.5,0.721687836487033));
#9813=CARTESIAN_POINT('',(1.25,11.85,-0.721687836487033));
#9814=CARTESIAN_POINT('',(1.25,10.5,0.721687836487033));
#9815=CARTESIAN_POINT('Origin',(-3.42958796722498E-16,10.5,1.44337567297406));
#9816=CARTESIAN_POINT('',(1.00899771935539E-14,10.5,1.44337567297406));
#9817=CARTESIAN_POINT('',(-3.42958796722498E-16,11.85,1.44337567297406));
#9818=CARTESIAN_POINT('',(-3.42958796722498E-16,10.5,1.44337567297406));
#9819=CARTESIAN_POINT('',(1.25,11.85,0.721687836487033));
#9820=CARTESIAN_POINT('',(-3.42958796722498E-16,10.5,1.44337567297406));
#9821=CARTESIAN_POINT('Origin',(-1.25,10.5,0.721687836487032));
#9822=CARTESIAN_POINT('',(-1.25,10.5,0.721687836487038));
#9823=CARTESIAN_POINT('',(-1.25,11.85,0.721687836487032));
#9824=CARTESIAN_POINT('',(-1.25,10.5,0.721687836487032));
#9825=CARTESIAN_POINT('',(-3.3881317890172E-16,11.85,1.44337567297406));
#9826=CARTESIAN_POINT('',(-1.25,10.5,0.721687836487032));
#9827=CARTESIAN_POINT('Origin',(-1.25,10.5,-0.721687836487033));
#9828=CARTESIAN_POINT('',(-1.25,10.5,-0.721687836487029));
#9829=CARTESIAN_POINT('',(-1.25,11.85,-0.721687836487033));
#9830=CARTESIAN_POINT('',(-1.25,10.5,-0.721687836487033));
#9831=CARTESIAN_POINT('',(-1.25,11.85,0.721687836487032));
#9832=CARTESIAN_POINT('',(-1.25,10.5,-0.721687836487033));
#9833=CARTESIAN_POINT('Origin',(-1.09387392956801E-17,10.5,-1.44337567297407));
#9834=CARTESIAN_POINT('',(-1.25,11.85,-0.721687836487033));
#9835=CARTESIAN_POINT('',(-1.09387392956801E-17,10.5,-1.44337567297407));
#9836=CARTESIAN_POINT('Origin',(1.25,11.85,0.721687836487033));
#9837=CARTESIAN_POINT('',(0.892857142857145,11.4928571428571,0.515491311776453));
#9838=CARTESIAN_POINT('',(0.892857142857144,11.4928571428571,-0.515491311776453));
#9839=CARTESIAN_POINT('Origin',(1.25,11.85,-0.721687836487033));
#9840=CARTESIAN_POINT('',(-4.33680868994202E-16,11.4928571428572,-1.03098262355291));
#9841=CARTESIAN_POINT('Origin',(-3.42958796722498E-16,11.85,1.44337567297406));
#9842=CARTESIAN_POINT('',(1.0842021724855E-15,11.4928571428572,1.03098262355291));
#9843=CARTESIAN_POINT('Origin',(-1.09387392956801E-17,11.85,-1.44337567297407));
#9844=CARTESIAN_POINT('',(-1.25,11.85,-0.721687836487033));
#9845=CARTESIAN_POINT('Origin',(-1.25,11.85,0.721687836487032));
#9846=CARTESIAN_POINT('',(-0.892857142857144,11.4928571428571,0.515491311776451));
#9847=CARTESIAN_POINT('Origin',(-1.25,11.85,-0.721687836487033));
#9848=CARTESIAN_POINT('Origin',(1.24999999999999,10.5,-0.721687836487047));
#9849=CARTESIAN_POINT('',(1.3661829762134E-15,10.3,-1.04337567297406));
#9850=CARTESIAN_POINT('',(2.38524477946811E-15,10.2113248654052,-0.866025403784446));
#9851=CARTESIAN_POINT('',(0.903589838486216,10.3,-0.521687836487043));
#9852=CARTESIAN_POINT('',(0.451794919243109,10.3,-0.782531754730552));
#9853=CARTESIAN_POINT('',(0.749999999999994,10.2113248654052,-0.43301270189223));
#9854=CARTESIAN_POINT('Origin',(1.25000000000001,10.5,0.721687836487021));
#9855=CARTESIAN_POINT('',(0.903589838486227,10.3,0.521687836487022));
#9856=CARTESIAN_POINT('',(0.903589838486221,10.3,-9.50233343939879E-15));
#9857=CARTESIAN_POINT('',(0.750000000000001,10.2113248654052,0.433012701892211));
#9858=CARTESIAN_POINT('Origin',(1.00899771935539E-14,10.5,1.44337567297406));
#9859=CARTESIAN_POINT('',(7.27313732092168E-15,10.3,1.04337567297406));
#9860=CARTESIAN_POINT('',(0.451794919243117,10.3,0.782531754730542));
#9861=CARTESIAN_POINT('',(6.28837260041593E-15,10.2113248654052,0.866025403784435));
#9862=CARTESIAN_POINT('Origin',(-1.25,10.5,0.721687836487038));
#9863=CARTESIAN_POINT('',(-0.90358983848622,10.3,0.521687836487035));
#9864=CARTESIAN_POINT('',(-0.451794919243106,10.3,0.782531754730548));
#9865=CARTESIAN_POINT('',(-0.749999999999995,10.2113248654052,0.433012701892221));
#9866=CARTESIAN_POINT('Origin',(-1.25,10.5,-0.721687836487029));
#9867=CARTESIAN_POINT('',(-0.903589838486223,10.3,-0.521687836487029));
#9868=CARTESIAN_POINT('',(-0.903589838486221,10.3,2.98644765238248E-15));
#9869=CARTESIAN_POINT('',(-0.749999999999998,10.2113248654052,-0.433012701892216));
#9870=CARTESIAN_POINT('Origin',(-1.09387392956801E-17,10.5,-1.44337567297407));
#9871=CARTESIAN_POINT('',(-0.451794919243112,10.3,-0.782531754730545));
#9872=CARTESIAN_POINT('Origin',(0.,10.3,0.));
#9873=CARTESIAN_POINT('',(-1.11448938007103,-0.584501651924837,12.));
#9874=CARTESIAN_POINT('',(-1.11448938007103,-0.584501651924837,-11.));
#9875=CARTESIAN_POINT('',(-1.11448938007103,-0.584501651924837,24.0000000000063));
#9876=CARTESIAN_POINT('',(-1.11448938007103,-0.584501651924837,41.));
#9877=CARTESIAN_POINT('',(-1.11448938007155,1.91549834807536,46.));
#9878=CARTESIAN_POINT('',(-18.1144893800717,4.41549834807508,52.9534192652434));
#9879=CARTESIAN_POINT('',(-12.1144893800717,10.9154983480751,3.07000000000636));
#9880=CARTESIAN_POINT('',(-1.11448938007103,-0.584501651924837,7.00000000000635));
#9881=CARTESIAN_POINT('',(-1.11448938007102,1.91549834807516,2.00000000000636));
#9882=CARTESIAN_POINT('',(-18.1144893800717,4.41549834807508,-6.99999999999365));
#9883=CARTESIAN_POINT('',(9.88551061992831,10.9154983480751,2.94500000000636));
#9884=CARTESIAN_POINT('',(-12.1144893800717,10.9154983480751,44.8834192652434));
#9885=CARTESIAN_POINT('',(9.88551061992831,10.9154983480751,45.0084192652434));
#9886=UNCERTAINTY_MEASURE_WITH_UNIT(LENGTH_MEASURE(0.01),#9904,
'DISTANCE_ACCURACY_VALUE',
'Maximum model space distance between geometric entities at asserted c
onnectivities');
#9887=UNCERTAINTY_MEASURE_WITH_UNIT(LENGTH_MEASURE(0.01),#9904,
'DISTANCE_ACCURACY_VALUE',
'Maximum model space distance between geometric entities at asserted c
onnectivities');
#9888=UNCERTAINTY_MEASURE_WITH_UNIT(LENGTH_MEASURE(0.01),#9904,
'DISTANCE_ACCURACY_VALUE',
'Maximum model space distance between geometric entities at asserted c
onnectivities');
#9889=UNCERTAINTY_MEASURE_WITH_UNIT(LENGTH_MEASURE(0.01),#9904,
'DISTANCE_ACCURACY_VALUE',
'Maximum model space distance between geometric entities at asserted c
onnectivities');
#9890=UNCERTAINTY_MEASURE_WITH_UNIT(LENGTH_MEASURE(0.01),#9904,
'DISTANCE_ACCURACY_VALUE',
'Maximum model space distance between geometric entities at asserted c
onnectivities');
#9891=UNCERTAINTY_MEASURE_WITH_UNIT(LENGTH_MEASURE(0.01),#9904,
'DISTANCE_ACCURACY_VALUE',
'Maximum model space distance between geometric entities at asserted c
onnectivities');
#9892=UNCERTAINTY_MEASURE_WITH_UNIT(LENGTH_MEASURE(0.01),#9904,
'DISTANCE_ACCURACY_VALUE',
'Maximum model space distance between geometric entities at asserted c
onnectivities');
#9893=UNCERTAINTY_MEASURE_WITH_UNIT(LENGTH_MEASURE(0.01),#9904,
'DISTANCE_ACCURACY_VALUE',
'Maximum model space distance between geometric entities at asserted c
onnectivities');
#9894=UNCERTAINTY_MEASURE_WITH_UNIT(LENGTH_MEASURE(0.01),#9904,
'DISTANCE_ACCURACY_VALUE',
'Maximum model space distance between geometric entities at asserted c
onnectivities');
#9895=(
GEOMETRIC_REPRESENTATION_CONTEXT(3)
GLOBAL_UNCERTAINTY_ASSIGNED_CONTEXT((#9886))
GLOBAL_UNIT_ASSIGNED_CONTEXT((#9904,#9906,#9907))
REPRESENTATION_CONTEXT('','3D')
);
#9896=(
GEOMETRIC_REPRESENTATION_CONTEXT(3)
GLOBAL_UNCERTAINTY_ASSIGNED_CONTEXT((#9887))
GLOBAL_UNIT_ASSIGNED_CONTEXT((#9904,#9906,#9907))
REPRESENTATION_CONTEXT('','3D')
);
#9897=(
GEOMETRIC_REPRESENTATION_CONTEXT(3)
GLOBAL_UNCERTAINTY_ASSIGNED_CONTEXT((#9888))
GLOBAL_UNIT_ASSIGNED_CONTEXT((#9904,#9906,#9907))
REPRESENTATION_CONTEXT('','3D')
);
#9898=(
GEOMETRIC_REPRESENTATION_CONTEXT(3)
GLOBAL_UNCERTAINTY_ASSIGNED_CONTEXT((#9889))
GLOBAL_UNIT_ASSIGNED_CONTEXT((#9904,#9906,#9907))
REPRESENTATION_CONTEXT('','3D')
);
#9899=(
GEOMETRIC_REPRESENTATION_CONTEXT(3)
GLOBAL_UNCERTAINTY_ASSIGNED_CONTEXT((#9890))
GLOBAL_UNIT_ASSIGNED_CONTEXT((#9904,#9906,#9907))
REPRESENTATION_CONTEXT('','3D')
);
#9900=(
GEOMETRIC_REPRESENTATION_CONTEXT(3)
GLOBAL_UNCERTAINTY_ASSIGNED_CONTEXT((#9891))
GLOBAL_UNIT_ASSIGNED_CONTEXT((#9904,#9906,#9907))
REPRESENTATION_CONTEXT('','3D')
);
#9901=(
GEOMETRIC_REPRESENTATION_CONTEXT(3)
GLOBAL_UNCERTAINTY_ASSIGNED_CONTEXT((#9892))
GLOBAL_UNIT_ASSIGNED_CONTEXT((#9904,#9906,#9907))
REPRESENTATION_CONTEXT('','3D')
);
#9902=(
GEOMETRIC_REPRESENTATION_CONTEXT(3)
GLOBAL_UNCERTAINTY_ASSIGNED_CONTEXT((#9893))
GLOBAL_UNIT_ASSIGNED_CONTEXT((#9904,#9906,#9907))
REPRESENTATION_CONTEXT('','3D')
);
#9903=(
GEOMETRIC_REPRESENTATION_CONTEXT(3)
GLOBAL_UNCERTAINTY_ASSIGNED_CONTEXT((#9894))
GLOBAL_UNIT_ASSIGNED_CONTEXT((#9904,#9906,#9907))
REPRESENTATION_CONTEXT('','3D')
);
#9904=(
LENGTH_UNIT()
NAMED_UNIT(*)
SI_UNIT(.MILLI.,.METRE.)
);
#9905=(
LENGTH_UNIT()
NAMED_UNIT(*)
SI_UNIT($,.METRE.)
);
#9906=(
NAMED_UNIT(*)
PLANE_ANGLE_UNIT()
SI_UNIT($,.RADIAN.)
);
#9907=(
NAMED_UNIT(*)
SI_UNIT($,.STERADIAN.)
SOLID_ANGLE_UNIT()
);
#9908=SHAPE_DEFINITION_REPRESENTATION(#9916,#9937);
#9909=SHAPE_DEFINITION_REPRESENTATION(#9917,#9938);
#9910=SHAPE_DEFINITION_REPRESENTATION(#9918,#9939);
#9911=SHAPE_DEFINITION_REPRESENTATION(#9919,#9940);
#9912=SHAPE_DEFINITION_REPRESENTATION(#9920,#9941);
#9913=SHAPE_DEFINITION_REPRESENTATION(#9921,#9942);
#9914=SHAPE_DEFINITION_REPRESENTATION(#9922,#9943);
#9915=SHAPE_DEFINITION_REPRESENTATION(#9923,#9944);
#9916=PRODUCT_DEFINITION_SHAPE('',$,#9946);
#9917=PRODUCT_DEFINITION_SHAPE('',$,#9947);
#9918=PRODUCT_DEFINITION_SHAPE('',$,#9948);
#9919=PRODUCT_DEFINITION_SHAPE('',$,#9949);
#9920=PRODUCT_DEFINITION_SHAPE('',$,#9950);
#9921=PRODUCT_DEFINITION_SHAPE('',$,#9951);
#9922=PRODUCT_DEFINITION_SHAPE('',$,#9952);
#9923=PRODUCT_DEFINITION_SHAPE('',$,#9953);
#9924=PRODUCT_DEFINITION_SHAPE($,$,#50);
#9925=PRODUCT_DEFINITION_SHAPE($,$,#51);
#9926=PRODUCT_DEFINITION_SHAPE($,$,#52);
#9927=PRODUCT_DEFINITION_SHAPE($,$,#53);
#9928=PRODUCT_DEFINITION_SHAPE($,$,#54);
#9929=PRODUCT_DEFINITION_SHAPE($,$,#55);
#9930=PRODUCT_DEFINITION_SHAPE($,$,#56);
#9931=PRODUCT_DEFINITION_SHAPE($,$,#57);
#9932=PRODUCT_DEFINITION_SHAPE($,$,#58);
#9933=PRODUCT_DEFINITION_SHAPE($,$,#59);
#9934=PRODUCT_DEFINITION_SHAPE($,$,#60);
#9935=PRODUCT_DEFINITION_SHAPE($,$,#61);
#9936=PRODUCT_DEFINITION_SHAPE($,$,#62);
#9937=SHAPE_REPRESENTATION('',(#2107,#2305,#2306,#2307,#2308,#2309,#2310,
#2311,#2312,#2313,#2314,#2315,#2316,#2317),#9895);
#9938=SHAPE_REPRESENTATION('',(#2108),#9896);
#9939=SHAPE_REPRESENTATION('',(#2117),#9897);
#9940=SHAPE_REPRESENTATION('',(#2141),#9898);
#9941=SHAPE_REPRESENTATION('',(#2189),#9899);
#9942=SHAPE_REPRESENTATION('',(#2198),#9900);
#9943=SHAPE_REPRESENTATION('',(#2221),#9901);
#9944=SHAPE_REPRESENTATION('',(#2234),#9902);
#9945=PRODUCT_DEFINITION_CONTEXT('part definition',#9971,'design');
#9946=PRODUCT_DEFINITION('MAT-010','MAT-010',#9954,#9945);
#9947=PRODUCT_DEFINITION('bushing','Bushing',#9955,#9945);
#9948=PRODUCT_DEFINITION('Axle','Axle',#9956,#9945);
#9949=PRODUCT_DEFINITION('pulley','Pulley',#9957,#9945);
#9950=PRODUCT_DEFINITION('Thrust washer','Thrust Washer',#9958,#9945);
#9951=PRODUCT_DEFINITION('U-Bracket','U-Bracket',#9959,#9945);
#9952=PRODUCT_DEFINITION('Retaining Plate','Retaining Plate',#9960,#9945);
#9953=PRODUCT_DEFINITION('Countersunk Screw ISO 10642 M4x12 A2',
'Countersunk Screw ISO 10642 M4x12 A2',#9961,#9945);
#9954=PRODUCT_DEFINITION_FORMATION('',$,#9973);
#9955=PRODUCT_DEFINITION_FORMATION('',$,#9974);
#9956=PRODUCT_DEFINITION_FORMATION('',$,#9975);
#9957=PRODUCT_DEFINITION_FORMATION('',$,#9976);
#9958=PRODUCT_DEFINITION_FORMATION('',$,#9977);
#9959=PRODUCT_DEFINITION_FORMATION('',$,#9978);
#9960=PRODUCT_DEFINITION_FORMATION('',$,#9979);
#9961=PRODUCT_DEFINITION_FORMATION('',$,#9980);
#9962=PRODUCT_RELATED_PRODUCT_CATEGORY('MAT-010','MAT-010',(#9973));
#9963=PRODUCT_RELATED_PRODUCT_CATEGORY('Bushing','Bushing',(#9974));
#9964=PRODUCT_RELATED_PRODUCT_CATEGORY('Axle','Axle',(#9975));
#9965=PRODUCT_RELATED_PRODUCT_CATEGORY('Pulley','Pulley',(#9976));
#9966=PRODUCT_RELATED_PRODUCT_CATEGORY('Thrust Washer','Thrust Washer',
(#9977));
#9967=PRODUCT_RELATED_PRODUCT_CATEGORY('U-Bracket','U-Bracket',(#9978));
#9968=PRODUCT_RELATED_PRODUCT_CATEGORY('Retaining Plate',
'Retaining Plate',(#9979));
#9969=PRODUCT_RELATED_PRODUCT_CATEGORY(
'Countersunk Screw ISO 10642 M4x12 A2',
'Countersunk Screw ISO 10642 M4x12 A2',(#9980));
#9970=APPLICATION_PROTOCOL_DEFINITION('international standard',
'automotive_design',2009,#9971);
#9971=APPLICATION_CONTEXT(
'Core Data for Automotive Mechanical Design Process');
#9972=PRODUCT_CONTEXT('part definition',#9971,'mechanical');
#9973=PRODUCT('MAT-010','MAT-010','STEP AP214',(#9972));
#9974=PRODUCT('bushing','Bushing',$,(#9972));
#9975=PRODUCT('Axle','Axle',$,(#9972));
#9976=PRODUCT('pulley','Pulley',$,(#9972));
#9977=PRODUCT('Thrust washer','Thrust Washer',$,(#9972));
#9978=PRODUCT('U-Bracket','U-Bracket',$,(#9972));
#9979=PRODUCT('Retaining Plate','Retaining Plate',$,(#9972));
#9980=PRODUCT('Countersunk Screw ISO 10642 M4x12 A2',
'Countersunk Screw ISO 10642 M4x12 A2',$,(#9972));
#9981=PRESENTATION_STYLE_ASSIGNMENT((#9986));
#9982=PRESENTATION_STYLE_ASSIGNMENT((#9987));
#9983=PRESENTATION_STYLE_ASSIGNMENT((#9988));
#9984=PRESENTATION_STYLE_ASSIGNMENT((#9989));
#9985=PRESENTATION_STYLE_ASSIGNMENT((#9990));
#9986=SURFACE_STYLE_USAGE(.BOTH.,#9991);
#9987=SURFACE_STYLE_USAGE(.BOTH.,#9992);
#9988=SURFACE_STYLE_USAGE(.BOTH.,#9993);
#9989=SURFACE_STYLE_USAGE(.BOTH.,#9994);
#9990=SURFACE_STYLE_USAGE(.BOTH.,#9995);
#9991=SURFACE_SIDE_STYLE('',(#9996));
#9992=SURFACE_SIDE_STYLE('',(#9997));
#9993=SURFACE_SIDE_STYLE('',(#9998));
#9994=SURFACE_SIDE_STYLE('',(#9999));
#9995=SURFACE_SIDE_STYLE('',(#10000));
#9996=SURFACE_STYLE_FILL_AREA(#10001);
#9997=SURFACE_STYLE_FILL_AREA(#10002);
#9998=SURFACE_STYLE_FILL_AREA(#10003);
#9999=SURFACE_STYLE_FILL_AREA(#10004);
#10000=SURFACE_STYLE_FILL_AREA(#10005);
#10001=FILL_AREA_STYLE('Steel - Satin',(#10006));
#10002=FILL_AREA_STYLE('Opaque(97,158,199)',(#10007));
#10003=FILL_AREA_STYLE('Opaque(61,176,222)',(#10008));
#10004=FILL_AREA_STYLE('Opaque(227,224,212)',(#10009));
#10005=FILL_AREA_STYLE('Opaque(31,36,43)',(#10010));
#10006=FILL_AREA_STYLE_COLOUR('Steel - Satin',#10011);
#10007=FILL_AREA_STYLE_COLOUR('Opaque(97,158,199)',#10012);
#10008=FILL_AREA_STYLE_COLOUR('Opaque(61,176,222)',#10013);
#10009=FILL_AREA_STYLE_COLOUR('Opaque(227,224,212)',#10014);
#10010=FILL_AREA_STYLE_COLOUR('Opaque(31,36,43)',#10015);
#10011=COLOUR_RGB('Steel - Satin',0.627450980392157,0.627450980392157,0.627450980392157);
#10012=COLOUR_RGB('Opaque(97,158,199)',0.380392156862745,0.619607843137255,
0.780392156862745);
#10013=COLOUR_RGB('Opaque(61,176,222)',0.23921568627451,0.690196078431373,
0.870588235294118);
#10014=COLOUR_RGB('Opaque(227,224,212)',0.890196078431372,0.87843137254902,
0.831372549019608);
#10015=COLOUR_RGB('Opaque(31,36,43)',0.12156862745098,0.141176470588235,
0.168627450980392);
ENDSEC;
END-ISO-10303-21;
